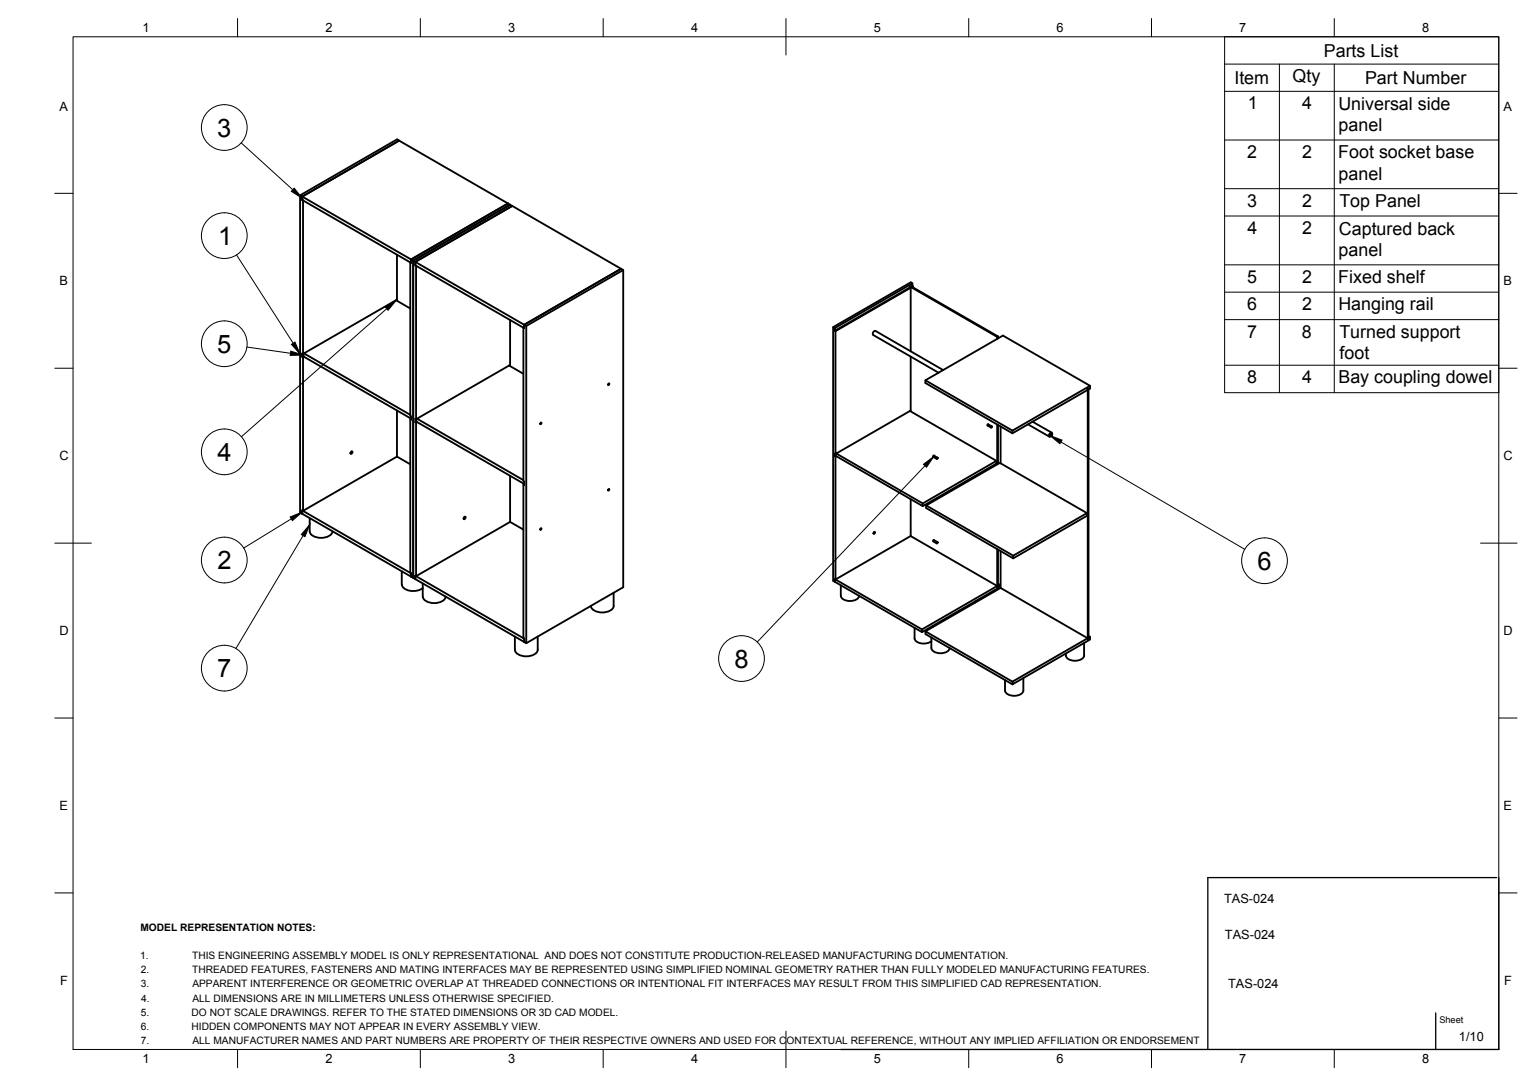
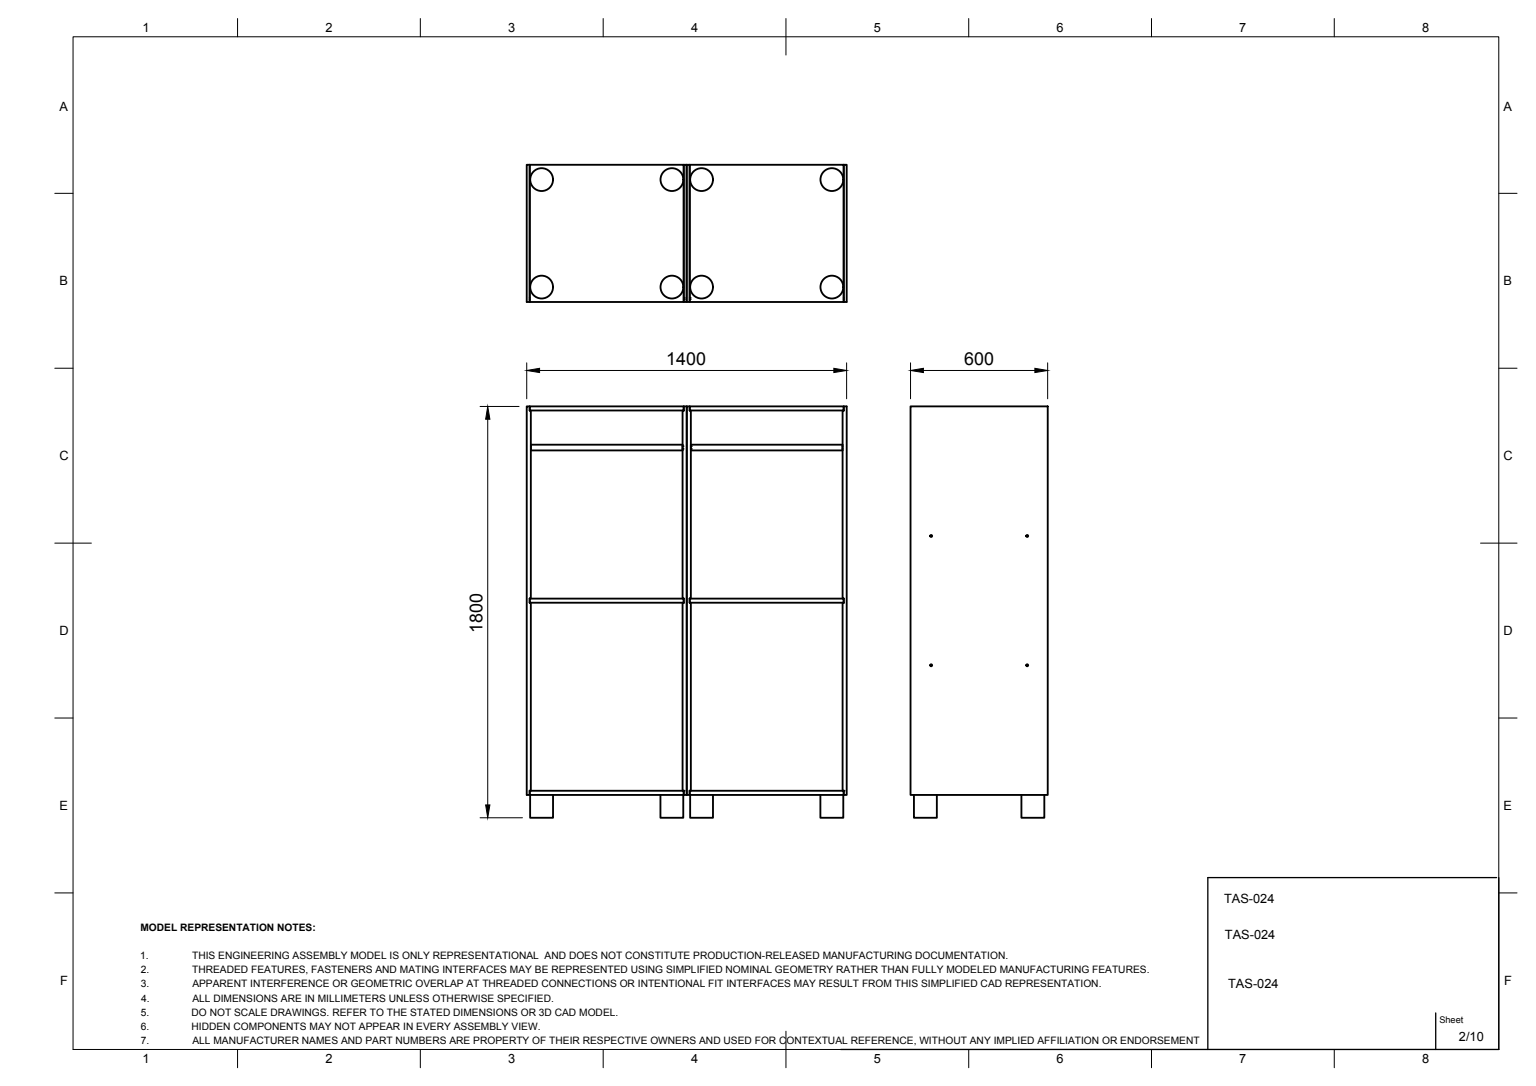
ISO-10303-21;
HEADER;
/* Generated by software containing ST-Developer
 * from STEP Tools, Inc. (www.steptools.com) 
 */

FILE_DESCRIPTION(
/* description */ (''),
/* implementation_level */ '2;1');

FILE_NAME(
/* name */ 'TAS-024.step',
/* time_stamp */ '2026-11-15T17:53:25-08:00',
/* author */ (''),
/* organization */ (''),
/* preprocessor_version */ 'ST-DEVELOPER v20.2',
/* originating_system */ 'Autodesk Translation Framework v15.17.0.0',
/* authorisation */ '');

FILE_SCHEMA (('AUTOMOTIVE_DESIGN { 1 0 10303 214 3 1 1 }'));
ENDSEC;

DATA;
#10=MECHANICAL_DESIGN_GEOMETRIC_PRESENTATION_REPRESENTATION('',(#131,#132,
#133,#134,#135,#136,#137,#138),#2673);
#11=ITEM_DEFINED_TRANSFORMATION($,$,#1615,#1744);
#12=ITEM_DEFINED_TRANSFORMATION($,$,#1662,#1745);
#13=ITEM_DEFINED_TRANSFORMATION($,$,#1689,#1746);
#14=ITEM_DEFINED_TRANSFORMATION($,$,#1700,#1747);
#15=ITEM_DEFINED_TRANSFORMATION($,$,#1707,#1748);
#16=ITEM_DEFINED_TRANSFORMATION($,$,#1714,#1749);
#17=ITEM_DEFINED_TRANSFORMATION($,$,#1728,#1750);
#18=ITEM_DEFINED_TRANSFORMATION($,$,#1738,#1751);
#19=ITEM_DEFINED_TRANSFORMATION($,$,#1615,#1752);
#20=ITEM_DEFINED_TRANSFORMATION($,$,#1728,#1753);
#21=ITEM_DEFINED_TRANSFORMATION($,$,#1728,#1754);
#22=ITEM_DEFINED_TRANSFORMATION($,$,#1728,#1755);
#23=ITEM_DEFINED_TRANSFORMATION($,$,#1615,#1756);
#24=ITEM_DEFINED_TRANSFORMATION($,$,#1615,#1757);
#25=ITEM_DEFINED_TRANSFORMATION($,$,#1662,#1758);
#26=ITEM_DEFINED_TRANSFORMATION($,$,#1689,#1759);
#27=ITEM_DEFINED_TRANSFORMATION($,$,#1700,#1760);
#28=ITEM_DEFINED_TRANSFORMATION($,$,#1707,#1761);
#29=ITEM_DEFINED_TRANSFORMATION($,$,#1714,#1762);
#30=ITEM_DEFINED_TRANSFORMATION($,$,#1728,#1763);
#31=ITEM_DEFINED_TRANSFORMATION($,$,#1728,#1764);
#32=ITEM_DEFINED_TRANSFORMATION($,$,#1728,#1765);
#33=ITEM_DEFINED_TRANSFORMATION($,$,#1728,#1766);
#34=ITEM_DEFINED_TRANSFORMATION($,$,#1738,#1767);
#35=ITEM_DEFINED_TRANSFORMATION($,$,#1738,#1768);
#36=ITEM_DEFINED_TRANSFORMATION($,$,#1738,#1769);
#37=(
REPRESENTATION_RELATIONSHIP($,$,#2723,#2722)
REPRESENTATION_RELATIONSHIP_WITH_TRANSFORMATION(#11)
SHAPE_REPRESENTATION_RELATIONSHIP()
);
#38=(
REPRESENTATION_RELATIONSHIP($,$,#2724,#2722)
REPRESENTATION_RELATIONSHIP_WITH_TRANSFORMATION(#12)
SHAPE_REPRESENTATION_RELATIONSHIP()
);
#39=(
REPRESENTATION_RELATIONSHIP($,$,#2725,#2722)
REPRESENTATION_RELATIONSHIP_WITH_TRANSFORMATION(#13)
SHAPE_REPRESENTATION_RELATIONSHIP()
);
#40=(
REPRESENTATION_RELATIONSHIP($,$,#2726,#2722)
REPRESENTATION_RELATIONSHIP_WITH_TRANSFORMATION(#14)
SHAPE_REPRESENTATION_RELATIONSHIP()
);
#41=(
REPRESENTATION_RELATIONSHIP($,$,#2727,#2722)
REPRESENTATION_RELATIONSHIP_WITH_TRANSFORMATION(#15)
SHAPE_REPRESENTATION_RELATIONSHIP()
);
#42=(
REPRESENTATION_RELATIONSHIP($,$,#2728,#2722)
REPRESENTATION_RELATIONSHIP_WITH_TRANSFORMATION(#16)
SHAPE_REPRESENTATION_RELATIONSHIP()
);
#43=(
REPRESENTATION_RELATIONSHIP($,$,#2729,#2722)
REPRESENTATION_RELATIONSHIP_WITH_TRANSFORMATION(#17)
SHAPE_REPRESENTATION_RELATIONSHIP()
);
#44=(
REPRESENTATION_RELATIONSHIP($,$,#2730,#2722)
REPRESENTATION_RELATIONSHIP_WITH_TRANSFORMATION(#18)
SHAPE_REPRESENTATION_RELATIONSHIP()
);
#45=(
REPRESENTATION_RELATIONSHIP($,$,#2723,#2722)
REPRESENTATION_RELATIONSHIP_WITH_TRANSFORMATION(#19)
SHAPE_REPRESENTATION_RELATIONSHIP()
);
#46=(
REPRESENTATION_RELATIONSHIP($,$,#2729,#2722)
REPRESENTATION_RELATIONSHIP_WITH_TRANSFORMATION(#20)
SHAPE_REPRESENTATION_RELATIONSHIP()
);
#47=(
REPRESENTATION_RELATIONSHIP($,$,#2729,#2722)
REPRESENTATION_RELATIONSHIP_WITH_TRANSFORMATION(#21)
SHAPE_REPRESENTATION_RELATIONSHIP()
);
#48=(
REPRESENTATION_RELATIONSHIP($,$,#2729,#2722)
REPRESENTATION_RELATIONSHIP_WITH_TRANSFORMATION(#22)
SHAPE_REPRESENTATION_RELATIONSHIP()
);
#49=(
REPRESENTATION_RELATIONSHIP($,$,#2723,#2722)
REPRESENTATION_RELATIONSHIP_WITH_TRANSFORMATION(#23)
SHAPE_REPRESENTATION_RELATIONSHIP()
);
#50=(
REPRESENTATION_RELATIONSHIP($,$,#2723,#2722)
REPRESENTATION_RELATIONSHIP_WITH_TRANSFORMATION(#24)
SHAPE_REPRESENTATION_RELATIONSHIP()
);
#51=(
REPRESENTATION_RELATIONSHIP($,$,#2724,#2722)
REPRESENTATION_RELATIONSHIP_WITH_TRANSFORMATION(#25)
SHAPE_REPRESENTATION_RELATIONSHIP()
);
#52=(
REPRESENTATION_RELATIONSHIP($,$,#2725,#2722)
REPRESENTATION_RELATIONSHIP_WITH_TRANSFORMATION(#26)
SHAPE_REPRESENTATION_RELATIONSHIP()
);
#53=(
REPRESENTATION_RELATIONSHIP($,$,#2726,#2722)
REPRESENTATION_RELATIONSHIP_WITH_TRANSFORMATION(#27)
SHAPE_REPRESENTATION_RELATIONSHIP()
);
#54=(
REPRESENTATION_RELATIONSHIP($,$,#2727,#2722)
REPRESENTATION_RELATIONSHIP_WITH_TRANSFORMATION(#28)
SHAPE_REPRESENTATION_RELATIONSHIP()
);
#55=(
REPRESENTATION_RELATIONSHIP($,$,#2728,#2722)
REPRESENTATION_RELATIONSHIP_WITH_TRANSFORMATION(#29)
SHAPE_REPRESENTATION_RELATIONSHIP()
);
#56=(
REPRESENTATION_RELATIONSHIP($,$,#2729,#2722)
REPRESENTATION_RELATIONSHIP_WITH_TRANSFORMATION(#30)
SHAPE_REPRESENTATION_RELATIONSHIP()
);
#57=(
REPRESENTATION_RELATIONSHIP($,$,#2729,#2722)
REPRESENTATION_RELATIONSHIP_WITH_TRANSFORMATION(#31)
SHAPE_REPRESENTATION_RELATIONSHIP()
);
#58=(
REPRESENTATION_RELATIONSHIP($,$,#2729,#2722)
REPRESENTATION_RELATIONSHIP_WITH_TRANSFORMATION(#32)
SHAPE_REPRESENTATION_RELATIONSHIP()
);
#59=(
REPRESENTATION_RELATIONSHIP($,$,#2729,#2722)
REPRESENTATION_RELATIONSHIP_WITH_TRANSFORMATION(#33)
SHAPE_REPRESENTATION_RELATIONSHIP()
);
#60=(
REPRESENTATION_RELATIONSHIP($,$,#2730,#2722)
REPRESENTATION_RELATIONSHIP_WITH_TRANSFORMATION(#34)
SHAPE_REPRESENTATION_RELATIONSHIP()
);
#61=(
REPRESENTATION_RELATIONSHIP($,$,#2730,#2722)
REPRESENTATION_RELATIONSHIP_WITH_TRANSFORMATION(#35)
SHAPE_REPRESENTATION_RELATIONSHIP()
);
#62=(
REPRESENTATION_RELATIONSHIP($,$,#2730,#2722)
REPRESENTATION_RELATIONSHIP_WITH_TRANSFORMATION(#36)
SHAPE_REPRESENTATION_RELATIONSHIP()
);
#63=CONTEXT_DEPENDENT_SHAPE_REPRESENTATION(#37,#2696);
#64=CONTEXT_DEPENDENT_SHAPE_REPRESENTATION(#38,#2697);
#65=CONTEXT_DEPENDENT_SHAPE_REPRESENTATION(#39,#2698);
#66=CONTEXT_DEPENDENT_SHAPE_REPRESENTATION(#40,#2699);
#67=CONTEXT_DEPENDENT_SHAPE_REPRESENTATION(#41,#2700);
#68=CONTEXT_DEPENDENT_SHAPE_REPRESENTATION(#42,#2701);
#69=CONTEXT_DEPENDENT_SHAPE_REPRESENTATION(#43,#2702);
#70=CONTEXT_DEPENDENT_SHAPE_REPRESENTATION(#44,#2703);
#71=CONTEXT_DEPENDENT_SHAPE_REPRESENTATION(#45,#2704);
#72=CONTEXT_DEPENDENT_SHAPE_REPRESENTATION(#46,#2705);
#73=CONTEXT_DEPENDENT_SHAPE_REPRESENTATION(#47,#2706);
#74=CONTEXT_DEPENDENT_SHAPE_REPRESENTATION(#48,#2707);
#75=CONTEXT_DEPENDENT_SHAPE_REPRESENTATION(#49,#2708);
#76=CONTEXT_DEPENDENT_SHAPE_REPRESENTATION(#50,#2709);
#77=CONTEXT_DEPENDENT_SHAPE_REPRESENTATION(#51,#2710);
#78=CONTEXT_DEPENDENT_SHAPE_REPRESENTATION(#52,#2711);
#79=CONTEXT_DEPENDENT_SHAPE_REPRESENTATION(#53,#2712);
#80=CONTEXT_DEPENDENT_SHAPE_REPRESENTATION(#54,#2713);
#81=CONTEXT_DEPENDENT_SHAPE_REPRESENTATION(#55,#2714);
#82=CONTEXT_DEPENDENT_SHAPE_REPRESENTATION(#56,#2715);
#83=CONTEXT_DEPENDENT_SHAPE_REPRESENTATION(#57,#2716);
#84=CONTEXT_DEPENDENT_SHAPE_REPRESENTATION(#58,#2717);
#85=CONTEXT_DEPENDENT_SHAPE_REPRESENTATION(#59,#2718);
#86=CONTEXT_DEPENDENT_SHAPE_REPRESENTATION(#60,#2719);
#87=CONTEXT_DEPENDENT_SHAPE_REPRESENTATION(#61,#2720);
#88=CONTEXT_DEPENDENT_SHAPE_REPRESENTATION(#62,#2721);
#89=NEXT_ASSEMBLY_USAGE_OCCURRENCE('Universal side panel:1',
'Universal side panel:1','Universal side panel:1',#2732,#2733,
'Universal side panel:1');
#90=NEXT_ASSEMBLY_USAGE_OCCURRENCE('Foot socket base panel:1',
'Foot socket base panel:1','Foot socket base panel:1',#2732,#2734,
'Foot socket base panel:1');
#91=NEXT_ASSEMBLY_USAGE_OCCURRENCE('Top panel:1','Top panel:1',
'Top panel:1',#2732,#2735,'Top panel:1');
#92=NEXT_ASSEMBLY_USAGE_OCCURRENCE('Captured back panel:1',
'Captured back panel:1','Captured back panel:1',#2732,#2736,
'Captured back panel:1');
#93=NEXT_ASSEMBLY_USAGE_OCCURRENCE('Fixed shelf:1','Fixed shelf:1',
'Fixed shelf:1',#2732,#2737,'Fixed shelf:1');
#94=NEXT_ASSEMBLY_USAGE_OCCURRENCE('Hanging rail:1','Hanging rail:1',
'Hanging rail:1',#2732,#2738,'Hanging rail:1');
#95=NEXT_ASSEMBLY_USAGE_OCCURRENCE('Turned support foot:1',
'Turned support foot:1','Turned support foot:1',#2732,#2739,
'Turned support foot:1');
#96=NEXT_ASSEMBLY_USAGE_OCCURRENCE('Bay coupling dowel:1',
'Bay coupling dowel:1','Bay coupling dowel:1',#2732,#2740,
'Bay coupling dowel:1');
#97=NEXT_ASSEMBLY_USAGE_OCCURRENCE('Universal side panel:2',
'Universal side panel:2','Universal side panel:2',#2732,#2733,
'Universal side panel:2');
#98=NEXT_ASSEMBLY_USAGE_OCCURRENCE('Turned support foot:2',
'Turned support foot:2','Turned support foot:2',#2732,#2739,
'Turned support foot:2');
#99=NEXT_ASSEMBLY_USAGE_OCCURRENCE('Turned support foot:3',
'Turned support foot:3','Turned support foot:3',#2732,#2739,
'Turned support foot:3');
#100=NEXT_ASSEMBLY_USAGE_OCCURRENCE('Turned support foot:4',
'Turned support foot:4','Turned support foot:4',#2732,#2739,
'Turned support foot:4');
#101=NEXT_ASSEMBLY_USAGE_OCCURRENCE('Universal side panel:3',
'Universal side panel:3','Universal side panel:3',#2732,#2733,
'Universal side panel:3');
#102=NEXT_ASSEMBLY_USAGE_OCCURRENCE('Universal side panel:4',
'Universal side panel:4','Universal side panel:4',#2732,#2733,
'Universal side panel:4');
#103=NEXT_ASSEMBLY_USAGE_OCCURRENCE('Foot socket base panel:2',
'Foot socket base panel:2','Foot socket base panel:2',#2732,#2734,
'Foot socket base panel:2');
#104=NEXT_ASSEMBLY_USAGE_OCCURRENCE('Top panel:2','Top panel:2',
'Top panel:2',#2732,#2735,'Top panel:2');
#105=NEXT_ASSEMBLY_USAGE_OCCURRENCE('Captured back panel:2',
'Captured back panel:2','Captured back panel:2',#2732,#2736,
'Captured back panel:2');
#106=NEXT_ASSEMBLY_USAGE_OCCURRENCE('Fixed shelf:2','Fixed shelf:2',
'Fixed shelf:2',#2732,#2737,'Fixed shelf:2');
#107=NEXT_ASSEMBLY_USAGE_OCCURRENCE('Hanging rail:2','Hanging rail:2',
'Hanging rail:2',#2732,#2738,'Hanging rail:2');
#108=NEXT_ASSEMBLY_USAGE_OCCURRENCE('Turned support foot:5',
'Turned support foot:5','Turned support foot:5',#2732,#2739,
'Turned support foot:5');
#109=NEXT_ASSEMBLY_USAGE_OCCURRENCE('Turned support foot:6',
'Turned support foot:6','Turned support foot:6',#2732,#2739,
'Turned support foot:6');
#110=NEXT_ASSEMBLY_USAGE_OCCURRENCE('Turned support foot:7',
'Turned support foot:7','Turned support foot:7',#2732,#2739,
'Turned support foot:7');
#111=NEXT_ASSEMBLY_USAGE_OCCURRENCE('Turned support foot:8',
'Turned support foot:8','Turned support foot:8',#2732,#2739,
'Turned support foot:8');
#112=NEXT_ASSEMBLY_USAGE_OCCURRENCE('Bay coupling dowel:2',
'Bay coupling dowel:2','Bay coupling dowel:2',#2732,#2740,
'Bay coupling dowel:2');
#113=NEXT_ASSEMBLY_USAGE_OCCURRENCE('Bay coupling dowel:3',
'Bay coupling dowel:3','Bay coupling dowel:3',#2732,#2740,
'Bay coupling dowel:3');
#114=NEXT_ASSEMBLY_USAGE_OCCURRENCE('Bay coupling dowel:4',
'Bay coupling dowel:4','Bay coupling dowel:4',#2732,#2740,
'Bay coupling dowel:4');
#115=SHAPE_REPRESENTATION_RELATIONSHIP('SRR','None',#2723,#123);
#116=SHAPE_REPRESENTATION_RELATIONSHIP('SRR','None',#2724,#124);
#117=SHAPE_REPRESENTATION_RELATIONSHIP('SRR','None',#2725,#125);
#118=SHAPE_REPRESENTATION_RELATIONSHIP('SRR','None',#2726,#126);
#119=SHAPE_REPRESENTATION_RELATIONSHIP('SRR','None',#2727,#127);
#120=SHAPE_REPRESENTATION_RELATIONSHIP('SRR','None',#2728,#128);
#121=SHAPE_REPRESENTATION_RELATIONSHIP('SRR','None',#2729,#129);
#122=SHAPE_REPRESENTATION_RELATIONSHIP('SRR','None',#2730,#130);
#123=ADVANCED_BREP_SHAPE_REPRESENTATION('',(#139),#2665);
#124=ADVANCED_BREP_SHAPE_REPRESENTATION('',(#140),#2666);
#125=ADVANCED_BREP_SHAPE_REPRESENTATION('',(#141),#2667);
#126=ADVANCED_BREP_SHAPE_REPRESENTATION('',(#142),#2668);
#127=ADVANCED_BREP_SHAPE_REPRESENTATION('',(#143),#2669);
#128=ADVANCED_BREP_SHAPE_REPRESENTATION('',(#144),#2670);
#129=ADVANCED_BREP_SHAPE_REPRESENTATION('',(#145),#2671);
#130=ADVANCED_BREP_SHAPE_REPRESENTATION('',(#146),#2672);
#131=STYLED_ITEM('',(#2772),#139);
#132=STYLED_ITEM('',(#2773),#140);
#133=STYLED_ITEM('',(#2774),#141);
#134=STYLED_ITEM('',(#2775),#142);
#135=STYLED_ITEM('',(#2776),#143);
#136=STYLED_ITEM('',(#2777),#144);
#137=STYLED_ITEM('',(#2778),#145);
#138=STYLED_ITEM('',(#2779),#146);
#139=MANIFOLD_SOLID_BREP('Body1',#1517);
#140=MANIFOLD_SOLID_BREP('Body1',#1518);
#141=MANIFOLD_SOLID_BREP('Body1',#1519);
#142=MANIFOLD_SOLID_BREP('Body1',#1520);
#143=MANIFOLD_SOLID_BREP('Body1',#1521);
#144=MANIFOLD_SOLID_BREP('Body1',#1522);
#145=MANIFOLD_SOLID_BREP('Body1',#1523);
#146=MANIFOLD_SOLID_BREP('Body1',#1524);
#147=FACE_BOUND('',#342,.T.);
#148=FACE_BOUND('',#349,.T.);
#149=FACE_BOUND('',#357,.T.);
#150=FACE_BOUND('',#358,.T.);
#151=FACE_BOUND('',#359,.T.);
#152=FACE_BOUND('',#360,.T.);
#153=FACE_BOUND('',#380,.T.);
#154=FACE_BOUND('',#381,.T.);
#155=FACE_BOUND('',#382,.T.);
#156=FACE_BOUND('',#383,.T.);
#157=FACE_BOUND('',#412,.T.);
#158=FACE_BOUND('',#414,.T.);
#159=FACE_BOUND('',#419,.T.);
#160=PLANE('',#1619);
#161=PLANE('',#1623);
#162=PLANE('',#1627);
#163=PLANE('',#1631);
#164=PLANE('',#1635);
#165=PLANE('',#1639);
#166=PLANE('',#1640);
#167=PLANE('',#1641);
#168=PLANE('',#1642);
#169=PLANE('',#1643);
#170=PLANE('',#1644);
#171=PLANE('',#1645);
#172=PLANE('',#1646);
#173=PLANE('',#1647);
#174=PLANE('',#1648);
#175=PLANE('',#1649);
#176=PLANE('',#1650);
#177=PLANE('',#1651);
#178=PLANE('',#1652);
#179=PLANE('',#1653);
#180=PLANE('',#1654);
#181=PLANE('',#1655);
#182=PLANE('',#1656);
#183=PLANE('',#1657);
#184=PLANE('',#1658);
#185=PLANE('',#1659);
#186=PLANE('',#1660);
#187=PLANE('',#1661);
#188=PLANE('',#1666);
#189=PLANE('',#1670);
#190=PLANE('',#1674);
#191=PLANE('',#1678);
#192=PLANE('',#1679);
#193=PLANE('',#1680);
#194=PLANE('',#1681);
#195=PLANE('',#1682);
#196=PLANE('',#1683);
#197=PLANE('',#1684);
#198=PLANE('',#1685);
#199=PLANE('',#1686);
#200=PLANE('',#1687);
#201=PLANE('',#1688);
#202=PLANE('',#1690);
#203=PLANE('',#1691);
#204=PLANE('',#1692);
#205=PLANE('',#1693);
#206=PLANE('',#1694);
#207=PLANE('',#1695);
#208=PLANE('',#1696);
#209=PLANE('',#1697);
#210=PLANE('',#1698);
#211=PLANE('',#1699);
#212=PLANE('',#1701);
#213=PLANE('',#1702);
#214=PLANE('',#1703);
#215=PLANE('',#1704);
#216=PLANE('',#1705);
#217=PLANE('',#1706);
#218=PLANE('',#1708);
#219=PLANE('',#1709);
#220=PLANE('',#1710);
#221=PLANE('',#1711);
#222=PLANE('',#1712);
#223=PLANE('',#1713);
#224=PLANE('',#1718);
#225=PLANE('',#1722);
#226=PLANE('',#1726);
#227=PLANE('',#1727);
#228=PLANE('',#1732);
#229=PLANE('',#1736);
#230=PLANE('',#1737);
#231=PLANE('',#1742);
#232=PLANE('',#1743);
#233=FACE_OUTER_BOUND('',#322,.T.);
#234=FACE_OUTER_BOUND('',#323,.T.);
#235=FACE_OUTER_BOUND('',#324,.T.);
#236=FACE_OUTER_BOUND('',#325,.T.);
#237=FACE_OUTER_BOUND('',#326,.T.);
#238=FACE_OUTER_BOUND('',#327,.T.);
#239=FACE_OUTER_BOUND('',#328,.T.);
#240=FACE_OUTER_BOUND('',#329,.T.);
#241=FACE_OUTER_BOUND('',#330,.T.);
#242=FACE_OUTER_BOUND('',#331,.T.);
#243=FACE_OUTER_BOUND('',#332,.T.);
#244=FACE_OUTER_BOUND('',#333,.T.);
#245=FACE_OUTER_BOUND('',#334,.T.);
#246=FACE_OUTER_BOUND('',#335,.T.);
#247=FACE_OUTER_BOUND('',#336,.T.);
#248=FACE_OUTER_BOUND('',#337,.T.);
#249=FACE_OUTER_BOUND('',#338,.T.);
#250=FACE_OUTER_BOUND('',#339,.T.);
#251=FACE_OUTER_BOUND('',#340,.T.);
#252=FACE_OUTER_BOUND('',#341,.T.);
#253=FACE_OUTER_BOUND('',#343,.T.);
#254=FACE_OUTER_BOUND('',#344,.T.);
#255=FACE_OUTER_BOUND('',#345,.T.);
#256=FACE_OUTER_BOUND('',#346,.T.);
#257=FACE_OUTER_BOUND('',#347,.T.);
#258=FACE_OUTER_BOUND('',#348,.T.);
#259=FACE_OUTER_BOUND('',#350,.T.);
#260=FACE_OUTER_BOUND('',#351,.T.);
#261=FACE_OUTER_BOUND('',#352,.T.);
#262=FACE_OUTER_BOUND('',#353,.T.);
#263=FACE_OUTER_BOUND('',#354,.T.);
#264=FACE_OUTER_BOUND('',#355,.T.);
#265=FACE_OUTER_BOUND('',#356,.T.);
#266=FACE_OUTER_BOUND('',#361,.T.);
#267=FACE_OUTER_BOUND('',#362,.T.);
#268=FACE_OUTER_BOUND('',#363,.T.);
#269=FACE_OUTER_BOUND('',#364,.T.);
#270=FACE_OUTER_BOUND('',#365,.T.);
#271=FACE_OUTER_BOUND('',#366,.T.);
#272=FACE_OUTER_BOUND('',#367,.T.);
#273=FACE_OUTER_BOUND('',#368,.T.);
#274=FACE_OUTER_BOUND('',#369,.T.);
#275=FACE_OUTER_BOUND('',#370,.T.);
#276=FACE_OUTER_BOUND('',#371,.T.);
#277=FACE_OUTER_BOUND('',#372,.T.);
#278=FACE_OUTER_BOUND('',#373,.T.);
#279=FACE_OUTER_BOUND('',#374,.T.);
#280=FACE_OUTER_BOUND('',#375,.T.);
#281=FACE_OUTER_BOUND('',#376,.T.);
#282=FACE_OUTER_BOUND('',#377,.T.);
#283=FACE_OUTER_BOUND('',#378,.T.);
#284=FACE_OUTER_BOUND('',#379,.T.);
#285=FACE_OUTER_BOUND('',#384,.T.);
#286=FACE_OUTER_BOUND('',#385,.T.);
#287=FACE_OUTER_BOUND('',#386,.T.);
#288=FACE_OUTER_BOUND('',#387,.T.);
#289=FACE_OUTER_BOUND('',#388,.T.);
#290=FACE_OUTER_BOUND('',#389,.T.);
#291=FACE_OUTER_BOUND('',#390,.T.);
#292=FACE_OUTER_BOUND('',#391,.T.);
#293=FACE_OUTER_BOUND('',#392,.T.);
#294=FACE_OUTER_BOUND('',#393,.T.);
#295=FACE_OUTER_BOUND('',#394,.T.);
#296=FACE_OUTER_BOUND('',#395,.T.);
#297=FACE_OUTER_BOUND('',#396,.T.);
#298=FACE_OUTER_BOUND('',#397,.T.);
#299=FACE_OUTER_BOUND('',#398,.T.);
#300=FACE_OUTER_BOUND('',#399,.T.);
#301=FACE_OUTER_BOUND('',#400,.T.);
#302=FACE_OUTER_BOUND('',#401,.T.);
#303=FACE_OUTER_BOUND('',#402,.T.);
#304=FACE_OUTER_BOUND('',#403,.T.);
#305=FACE_OUTER_BOUND('',#404,.T.);
#306=FACE_OUTER_BOUND('',#405,.T.);
#307=FACE_OUTER_BOUND('',#406,.T.);
#308=FACE_OUTER_BOUND('',#407,.T.);
#309=FACE_OUTER_BOUND('',#408,.T.);
#310=FACE_OUTER_BOUND('',#409,.T.);
#311=FACE_OUTER_BOUND('',#410,.T.);
#312=FACE_OUTER_BOUND('',#411,.T.);
#313=FACE_OUTER_BOUND('',#413,.T.);
#314=FACE_OUTER_BOUND('',#415,.T.);
#315=FACE_OUTER_BOUND('',#416,.T.);
#316=FACE_OUTER_BOUND('',#417,.T.);
#317=FACE_OUTER_BOUND('',#418,.T.);
#318=FACE_OUTER_BOUND('',#420,.T.);
#319=FACE_OUTER_BOUND('',#421,.T.);
#320=FACE_OUTER_BOUND('',#422,.T.);
#321=FACE_OUTER_BOUND('',#423,.T.);
#322=EDGE_LOOP('',(#1052,#1053,#1054,#1055));
#323=EDGE_LOOP('',(#1056));
#324=EDGE_LOOP('',(#1057,#1058,#1059,#1060));
#325=EDGE_LOOP('',(#1061));
#326=EDGE_LOOP('',(#1062,#1063,#1064,#1065));
#327=EDGE_LOOP('',(#1066));
#328=EDGE_LOOP('',(#1067,#1068,#1069,#1070));
#329=EDGE_LOOP('',(#1071));
#330=EDGE_LOOP('',(#1072,#1073,#1074,#1075));
#331=EDGE_LOOP('',(#1076));
#332=EDGE_LOOP('',(#1077,#1078,#1079,#1080));
#333=EDGE_LOOP('',(#1081));
#334=EDGE_LOOP('',(#1082,#1083,#1084,#1085));
#335=EDGE_LOOP('',(#1086,#1087,#1088,#1089));
#336=EDGE_LOOP('',(#1090,#1091,#1092,#1093));
#337=EDGE_LOOP('',(#1094,#1095,#1096,#1097));
#338=EDGE_LOOP('',(#1098,#1099,#1100,#1101,#1102,#1103,#1104,#1105,#1106,
#1107,#1108,#1109,#1110,#1111,#1112,#1113,#1114,#1115,#1116,#1117));
#339=EDGE_LOOP('',(#1118,#1119,#1120,#1121));
#340=EDGE_LOOP('',(#1122,#1123,#1124,#1125));
#341=EDGE_LOOP('',(#1126,#1127,#1128,#1129));
#342=EDGE_LOOP('',(#1130));
#343=EDGE_LOOP('',(#1131,#1132,#1133,#1134));
#344=EDGE_LOOP('',(#1135,#1136,#1137,#1138));
#345=EDGE_LOOP('',(#1139,#1140,#1141,#1142));
#346=EDGE_LOOP('',(#1143,#1144,#1145,#1146));
#347=EDGE_LOOP('',(#1147,#1148,#1149,#1150));
#348=EDGE_LOOP('',(#1151,#1152,#1153,#1154));
#349=EDGE_LOOP('',(#1155));
#350=EDGE_LOOP('',(#1156,#1157,#1158,#1159));
#351=EDGE_LOOP('',(#1160,#1161,#1162,#1163));
#352=EDGE_LOOP('',(#1164,#1165,#1166,#1167));
#353=EDGE_LOOP('',(#1168,#1169,#1170,#1171,#1172,#1173,#1174,#1175,#1176,
#1177,#1178,#1179));
#354=EDGE_LOOP('',(#1180,#1181,#1182,#1183));
#355=EDGE_LOOP('',(#1184,#1185,#1186,#1187,#1188,#1189,#1190,#1191,#1192,
#1193,#1194,#1195));
#356=EDGE_LOOP('',(#1196,#1197,#1198,#1199));
#357=EDGE_LOOP('',(#1200));
#358=EDGE_LOOP('',(#1201));
#359=EDGE_LOOP('',(#1202));
#360=EDGE_LOOP('',(#1203));
#361=EDGE_LOOP('',(#1204,#1205,#1206,#1207));
#362=EDGE_LOOP('',(#1208,#1209,#1210,#1211));
#363=EDGE_LOOP('',(#1212));
#364=EDGE_LOOP('',(#1213,#1214,#1215,#1216));
#365=EDGE_LOOP('',(#1217));
#366=EDGE_LOOP('',(#1218,#1219,#1220,#1221));
#367=EDGE_LOOP('',(#1222));
#368=EDGE_LOOP('',(#1223,#1224,#1225,#1226));
#369=EDGE_LOOP('',(#1227));
#370=EDGE_LOOP('',(#1228,#1229,#1230,#1231));
#371=EDGE_LOOP('',(#1232,#1233,#1234,#1235));
#372=EDGE_LOOP('',(#1236,#1237,#1238,#1239));
#373=EDGE_LOOP('',(#1240,#1241,#1242,#1243,#1244,#1245,#1246,#1247));
#374=EDGE_LOOP('',(#1248,#1249,#1250,#1251));
#375=EDGE_LOOP('',(#1252,#1253,#1254,#1255));
#376=EDGE_LOOP('',(#1256,#1257,#1258,#1259));
#377=EDGE_LOOP('',(#1260,#1261,#1262,#1263,#1264,#1265,#1266,#1267));
#378=EDGE_LOOP('',(#1268,#1269,#1270,#1271));
#379=EDGE_LOOP('',(#1272,#1273,#1274,#1275));
#380=EDGE_LOOP('',(#1276));
#381=EDGE_LOOP('',(#1277));
#382=EDGE_LOOP('',(#1278));
#383=EDGE_LOOP('',(#1279));
#384=EDGE_LOOP('',(#1280,#1281,#1282,#1283));
#385=EDGE_LOOP('',(#1284,#1285,#1286,#1287));
#386=EDGE_LOOP('',(#1288,#1289,#1290,#1291));
#387=EDGE_LOOP('',(#1292,#1293,#1294,#1295,#1296,#1297,#1298,#1299));
#388=EDGE_LOOP('',(#1300,#1301,#1302,#1303));
#389=EDGE_LOOP('',(#1304,#1305,#1306,#1307));
#390=EDGE_LOOP('',(#1308,#1309,#1310,#1311));
#391=EDGE_LOOP('',(#1312,#1313,#1314,#1315,#1316,#1317,#1318,#1319));
#392=EDGE_LOOP('',(#1320,#1321,#1322,#1323));
#393=EDGE_LOOP('',(#1324,#1325,#1326,#1327));
#394=EDGE_LOOP('',(#1328,#1329,#1330,#1331));
#395=EDGE_LOOP('',(#1332,#1333,#1334,#1335));
#396=EDGE_LOOP('',(#1336,#1337,#1338,#1339));
#397=EDGE_LOOP('',(#1340,#1341,#1342,#1343));
#398=EDGE_LOOP('',(#1344,#1345,#1346,#1347));
#399=EDGE_LOOP('',(#1348,#1349,#1350,#1351));
#400=EDGE_LOOP('',(#1352,#1353,#1354,#1355));
#401=EDGE_LOOP('',(#1356,#1357,#1358,#1359));
#402=EDGE_LOOP('',(#1360,#1361,#1362,#1363));
#403=EDGE_LOOP('',(#1364,#1365,#1366,#1367));
#404=EDGE_LOOP('',(#1368,#1369,#1370,#1371));
#405=EDGE_LOOP('',(#1372,#1373,#1374,#1375));
#406=EDGE_LOOP('',(#1376,#1377,#1378,#1379));
#407=EDGE_LOOP('',(#1380));
#408=EDGE_LOOP('',(#1381,#1382,#1383,#1384));
#409=EDGE_LOOP('',(#1385));
#410=EDGE_LOOP('',(#1386,#1387,#1388,#1389));
#411=EDGE_LOOP('',(#1390));
#412=EDGE_LOOP('',(#1391));
#413=EDGE_LOOP('',(#1392));
#414=EDGE_LOOP('',(#1393));
#415=EDGE_LOOP('',(#1394,#1395,#1396,#1397));
#416=EDGE_LOOP('',(#1398));
#417=EDGE_LOOP('',(#1399,#1400,#1401,#1402));
#418=EDGE_LOOP('',(#1403));
#419=EDGE_LOOP('',(#1404));
#420=EDGE_LOOP('',(#1405));
#421=EDGE_LOOP('',(#1406,#1407,#1408,#1409));
#422=EDGE_LOOP('',(#1410));
#423=EDGE_LOOP('',(#1411));
#424=LINE('',#2236,#572);
#425=LINE('',#2243,#573);
#426=LINE('',#2250,#574);
#427=LINE('',#2257,#575);
#428=LINE('',#2264,#576);
#429=LINE('',#2271,#577);
#430=LINE('',#2277,#578);
#431=LINE('',#2279,#579);
#432=LINE('',#2281,#580);
#433=LINE('',#2282,#581);
#434=LINE('',#2286,#582);
#435=LINE('',#2288,#583);
#436=LINE('',#2290,#584);
#437=LINE('',#2291,#585);
#438=LINE('',#2295,#586);
#439=LINE('',#2297,#587);
#440=LINE('',#2299,#588);
#441=LINE('',#2300,#589);
#442=LINE('',#2304,#590);
#443=LINE('',#2306,#591);
#444=LINE('',#2308,#592);
#445=LINE('',#2309,#593);
#446=LINE('',#2312,#594);
#447=LINE('',#2314,#595);
#448=LINE('',#2316,#596);
#449=LINE('',#2318,#597);
#450=LINE('',#2319,#598);
#451=LINE('',#2321,#599);
#452=LINE('',#2323,#600);
#453=LINE('',#2324,#601);
#454=LINE('',#2326,#602);
#455=LINE('',#2328,#603);
#456=LINE('',#2330,#604);
#457=LINE('',#2332,#605);
#458=LINE('',#2333,#606);
#459=LINE('',#2335,#607);
#460=LINE('',#2337,#608);
#461=LINE('',#2338,#609);
#462=LINE('',#2341,#610);
#463=LINE('',#2342,#611);
#464=LINE('',#2345,#612);
#465=LINE('',#2346,#613);
#466=LINE('',#2349,#614);
#467=LINE('',#2350,#615);
#468=LINE('',#2353,#616);
#469=LINE('',#2354,#617);
#470=LINE('',#2356,#618);
#471=LINE('',#2358,#619);
#472=LINE('',#2361,#620);
#473=LINE('',#2362,#621);
#474=LINE('',#2365,#622);
#475=LINE('',#2366,#623);
#476=LINE('',#2369,#624);
#477=LINE('',#2370,#625);
#478=LINE('',#2373,#626);
#479=LINE('',#2374,#627);
#480=LINE('',#2376,#628);
#481=LINE('',#2378,#629);
#482=LINE('',#2381,#630);
#483=LINE('',#2383,#631);
#484=LINE('',#2384,#632);
#485=LINE('',#2387,#633);
#486=LINE('',#2388,#634);
#487=LINE('',#2391,#635);
#488=LINE('',#2392,#636);
#489=LINE('',#2394,#637);
#490=LINE('',#2401,#638);
#491=LINE('',#2408,#639);
#492=LINE('',#2415,#640);
#493=LINE('',#2422,#641);
#494=LINE('',#2428,#642);
#495=LINE('',#2430,#643);
#496=LINE('',#2432,#644);
#497=LINE('',#2433,#645);
#498=LINE('',#2437,#646);
#499=LINE('',#2439,#647);
#500=LINE('',#2441,#648);
#501=LINE('',#2442,#649);
#502=LINE('',#2444,#650);
#503=LINE('',#2445,#651);
#504=LINE('',#2448,#652);
#505=LINE('',#2450,#653);
#506=LINE('',#2452,#654);
#507=LINE('',#2454,#655);
#508=LINE('',#2455,#656);
#509=LINE('',#2458,#657);
#510=LINE('',#2459,#658);
#511=LINE('',#2462,#659);
#512=LINE('',#2464,#660);
#513=LINE('',#2465,#661);
#514=LINE('',#2468,#662);
#515=LINE('',#2469,#663);
#516=LINE('',#2471,#664);
#517=LINE('',#2472,#665);
#518=LINE('',#2479,#666);
#519=LINE('',#2481,#667);
#520=LINE('',#2483,#668);
#521=LINE('',#2484,#669);
#522=LINE('',#2488,#670);
#523=LINE('',#2490,#671);
#524=LINE('',#2492,#672);
#525=LINE('',#2493,#673);
#526=LINE('',#2495,#674);
#527=LINE('',#2496,#675);
#528=LINE('',#2499,#676);
#529=LINE('',#2501,#677);
#530=LINE('',#2503,#678);
#531=LINE('',#2505,#679);
#532=LINE('',#2506,#680);
#533=LINE('',#2509,#681);
#534=LINE('',#2510,#682);
#535=LINE('',#2513,#683);
#536=LINE('',#2515,#684);
#537=LINE('',#2516,#685);
#538=LINE('',#2519,#686);
#539=LINE('',#2520,#687);
#540=LINE('',#2522,#688);
#541=LINE('',#2523,#689);
#542=LINE('',#2530,#690);
#543=LINE('',#2532,#691);
#544=LINE('',#2534,#692);
#545=LINE('',#2535,#693);
#546=LINE('',#2538,#694);
#547=LINE('',#2540,#695);
#548=LINE('',#2541,#696);
#549=LINE('',#2544,#697);
#550=LINE('',#2546,#698);
#551=LINE('',#2547,#699);
#552=LINE('',#2549,#700);
#553=LINE('',#2550,#701);
#554=LINE('',#2557,#702);
#555=LINE('',#2559,#703);
#556=LINE('',#2561,#704);
#557=LINE('',#2562,#705);
#558=LINE('',#2565,#706);
#559=LINE('',#2567,#707);
#560=LINE('',#2568,#708);
#561=LINE('',#2571,#709);
#562=LINE('',#2573,#710);
#563=LINE('',#2574,#711);
#564=LINE('',#2576,#712);
#565=LINE('',#2577,#713);
#566=LINE('',#2585,#714);
#567=LINE('',#2592,#715);
#568=LINE('',#2599,#716);
#569=LINE('',#2608,#717);
#570=LINE('',#2615,#718);
#571=LINE('',#2624,#719);
#572=VECTOR('',#1778,0.409999999999997);
#573=VECTOR('',#1787,0.409999999999997);
#574=VECTOR('',#1796,0.409999999999997);
#575=VECTOR('',#1805,0.409999999999997);
#576=VECTOR('',#1814,0.620000000000001);
#577=VECTOR('',#1823,0.620000000000005);
#578=VECTOR('',#1830,1.);
#579=VECTOR('',#1831,1.);
#580=VECTOR('',#1832,1.);
#581=VECTOR('',#1833,1.);
#582=VECTOR('',#1836,1.);
#583=VECTOR('',#1837,1.);
#584=VECTOR('',#1838,1.);
#585=VECTOR('',#1839,1.);
#586=VECTOR('',#1842,1.);
#587=VECTOR('',#1843,1.);
#588=VECTOR('',#1844,1.);
#589=VECTOR('',#1845,1.);
#590=VECTOR('',#1848,1.);
#591=VECTOR('',#1849,1.);
#592=VECTOR('',#1850,1.);
#593=VECTOR('',#1851,1.);
#594=VECTOR('',#1854,1.);
#595=VECTOR('',#1855,1.);
#596=VECTOR('',#1856,1.);
#597=VECTOR('',#1857,1.);
#598=VECTOR('',#1858,1.);
#599=VECTOR('',#1859,1.);
#600=VECTOR('',#1860,1.);
#601=VECTOR('',#1861,1.);
#602=VECTOR('',#1862,1.);
#603=VECTOR('',#1863,1.);
#604=VECTOR('',#1864,1.);
#605=VECTOR('',#1865,1.);
#606=VECTOR('',#1866,1.);
#607=VECTOR('',#1867,1.);
#608=VECTOR('',#1868,1.);
#609=VECTOR('',#1869,1.);
#610=VECTOR('',#1872,1.);
#611=VECTOR('',#1873,1.);
#612=VECTOR('',#1876,1.);
#613=VECTOR('',#1877,1.);
#614=VECTOR('',#1880,1.);
#615=VECTOR('',#1881,1.);
#616=VECTOR('',#1884,1.);
#617=VECTOR('',#1885,1.);
#618=VECTOR('',#1888,1.);
#619=VECTOR('',#1891,1.);
#620=VECTOR('',#1894,1.);
#621=VECTOR('',#1895,1.);
#622=VECTOR('',#1898,1.);
#623=VECTOR('',#1899,1.);
#624=VECTOR('',#1902,1.);
#625=VECTOR('',#1903,1.);
#626=VECTOR('',#1906,1.);
#627=VECTOR('',#1907,1.);
#628=VECTOR('',#1910,1.);
#629=VECTOR('',#1913,1.);
#630=VECTOR('',#1916,1.);
#631=VECTOR('',#1917,1.);
#632=VECTOR('',#1918,1.);
#633=VECTOR('',#1921,1.);
#634=VECTOR('',#1922,1.);
#635=VECTOR('',#1925,1.);
#636=VECTOR('',#1926,1.);
#637=VECTOR('',#1929,1.);
#638=VECTOR('',#1938,0.619999999999997);
#639=VECTOR('',#1947,0.62);
#640=VECTOR('',#1956,0.62);
#641=VECTOR('',#1965,0.619999999999997);
#642=VECTOR('',#1972,1.);
#643=VECTOR('',#1973,1.);
#644=VECTOR('',#1974,1.);
#645=VECTOR('',#1975,1.);
#646=VECTOR('',#1978,1.);
#647=VECTOR('',#1979,1.);
#648=VECTOR('',#1980,1.);
#649=VECTOR('',#1981,1.);
#650=VECTOR('',#1984,1.);
#651=VECTOR('',#1985,1.);
#652=VECTOR('',#1988,1.);
#653=VECTOR('',#1989,1.);
#654=VECTOR('',#1990,1.);
#655=VECTOR('',#1991,1.);
#656=VECTOR('',#1992,1.);
#657=VECTOR('',#1995,1.);
#658=VECTOR('',#1996,1.);
#659=VECTOR('',#1999,1.);
#660=VECTOR('',#2000,1.);
#661=VECTOR('',#2001,1.);
#662=VECTOR('',#2004,1.);
#663=VECTOR('',#2005,1.);
#664=VECTOR('',#2008,1.);
#665=VECTOR('',#2009,1.);
#666=VECTOR('',#2018,1.);
#667=VECTOR('',#2019,1.);
#668=VECTOR('',#2020,1.);
#669=VECTOR('',#2021,1.);
#670=VECTOR('',#2024,1.);
#671=VECTOR('',#2025,1.);
#672=VECTOR('',#2026,1.);
#673=VECTOR('',#2027,1.);
#674=VECTOR('',#2030,1.);
#675=VECTOR('',#2031,1.);
#676=VECTOR('',#2034,1.);
#677=VECTOR('',#2035,1.);
#678=VECTOR('',#2036,1.);
#679=VECTOR('',#2037,1.);
#680=VECTOR('',#2038,1.);
#681=VECTOR('',#2041,1.);
#682=VECTOR('',#2042,1.);
#683=VECTOR('',#2045,1.);
#684=VECTOR('',#2046,1.);
#685=VECTOR('',#2047,1.);
#686=VECTOR('',#2050,1.);
#687=VECTOR('',#2051,1.);
#688=VECTOR('',#2054,1.);
#689=VECTOR('',#2055,1.);
#690=VECTOR('',#2064,1.);
#691=VECTOR('',#2065,1.);
#692=VECTOR('',#2066,1.);
#693=VECTOR('',#2067,1.);
#694=VECTOR('',#2070,1.);
#695=VECTOR('',#2071,1.);
#696=VECTOR('',#2072,1.);
#697=VECTOR('',#2075,1.);
#698=VECTOR('',#2076,1.);
#699=VECTOR('',#2077,1.);
#700=VECTOR('',#2080,1.);
#701=VECTOR('',#2081,1.);
#702=VECTOR('',#2090,1.);
#703=VECTOR('',#2091,1.);
#704=VECTOR('',#2092,1.);
#705=VECTOR('',#2093,1.);
#706=VECTOR('',#2096,1.);
#707=VECTOR('',#2097,1.);
#708=VECTOR('',#2098,1.);
#709=VECTOR('',#2101,1.);
#710=VECTOR('',#2102,1.);
#711=VECTOR('',#2103,1.);
#712=VECTOR('',#2106,1.);
#713=VECTOR('',#2107,1.);
#714=VECTOR('',#2118,0.6);
#715=VECTOR('',#2127,0.6);
#716=VECTOR('',#2136,1.25);
#717=VECTOR('',#2149,0.6);
#718=VECTOR('',#2158,5.);
#719=VECTOR('',#2171,0.4);
#720=CIRCLE('',#1617,0.409999999999997);
#721=CIRCLE('',#1618,0.409999999999997);
#722=CIRCLE('',#1621,0.409999999999997);
#723=CIRCLE('',#1622,0.409999999999997);
#724=CIRCLE('',#1625,0.409999999999997);
#725=CIRCLE('',#1626,0.409999999999997);
#726=CIRCLE('',#1629,0.409999999999997);
#727=CIRCLE('',#1630,0.409999999999997);
#728=CIRCLE('',#1633,0.620000000000001);
#729=CIRCLE('',#1634,0.620000000000001);
#730=CIRCLE('',#1637,0.620000000000005);
#731=CIRCLE('',#1638,0.620000000000005);
#732=CIRCLE('',#1664,0.619999999999997);
#733=CIRCLE('',#1665,0.619999999999997);
#734=CIRCLE('',#1668,0.62);
#735=CIRCLE('',#1669,0.62);
#736=CIRCLE('',#1672,0.62);
#737=CIRCLE('',#1673,0.62);
#738=CIRCLE('',#1676,0.619999999999997);
#739=CIRCLE('',#1677,0.619999999999997);
#740=CIRCLE('',#1716,0.6);
#741=CIRCLE('',#1717,0.6);
#742=CIRCLE('',#1720,0.6);
#743=CIRCLE('',#1721,0.6);
#744=CIRCLE('',#1724,1.25);
#745=CIRCLE('',#1725,1.25);
#746=CIRCLE('',#1730,0.6);
#747=CIRCLE('',#1731,0.6);
#748=CIRCLE('',#1734,5.);
#749=CIRCLE('',#1735,5.);
#750=CIRCLE('',#1740,0.4);
#751=CIRCLE('',#1741,0.4);
#752=VERTEX_POINT('',#2233);
#753=VERTEX_POINT('',#2235);
#754=VERTEX_POINT('',#2240);
#755=VERTEX_POINT('',#2242);
#756=VERTEX_POINT('',#2247);
#757=VERTEX_POINT('',#2249);
#758=VERTEX_POINT('',#2254);
#759=VERTEX_POINT('',#2256);
#760=VERTEX_POINT('',#2261);
#761=VERTEX_POINT('',#2263);
#762=VERTEX_POINT('',#2268);
#763=VERTEX_POINT('',#2270);
#764=VERTEX_POINT('',#2275);
#765=VERTEX_POINT('',#2276);
#766=VERTEX_POINT('',#2278);
#767=VERTEX_POINT('',#2280);
#768=VERTEX_POINT('',#2284);
#769=VERTEX_POINT('',#2285);
#770=VERTEX_POINT('',#2287);
#771=VERTEX_POINT('',#2289);
#772=VERTEX_POINT('',#2293);
#773=VERTEX_POINT('',#2294);
#774=VERTEX_POINT('',#2296);
#775=VERTEX_POINT('',#2298);
#776=VERTEX_POINT('',#2302);
#777=VERTEX_POINT('',#2303);
#778=VERTEX_POINT('',#2305);
#779=VERTEX_POINT('',#2307);
#780=VERTEX_POINT('',#2311);
#781=VERTEX_POINT('',#2313);
#782=VERTEX_POINT('',#2315);
#783=VERTEX_POINT('',#2317);
#784=VERTEX_POINT('',#2320);
#785=VERTEX_POINT('',#2322);
#786=VERTEX_POINT('',#2325);
#787=VERTEX_POINT('',#2327);
#788=VERTEX_POINT('',#2329);
#789=VERTEX_POINT('',#2331);
#790=VERTEX_POINT('',#2334);
#791=VERTEX_POINT('',#2336);
#792=VERTEX_POINT('',#2340);
#793=VERTEX_POINT('',#2344);
#794=VERTEX_POINT('',#2348);
#795=VERTEX_POINT('',#2352);
#796=VERTEX_POINT('',#2360);
#797=VERTEX_POINT('',#2364);
#798=VERTEX_POINT('',#2368);
#799=VERTEX_POINT('',#2372);
#800=VERTEX_POINT('',#2380);
#801=VERTEX_POINT('',#2382);
#802=VERTEX_POINT('',#2386);
#803=VERTEX_POINT('',#2390);
#804=VERTEX_POINT('',#2398);
#805=VERTEX_POINT('',#2400);
#806=VERTEX_POINT('',#2405);
#807=VERTEX_POINT('',#2407);
#808=VERTEX_POINT('',#2412);
#809=VERTEX_POINT('',#2414);
#810=VERTEX_POINT('',#2419);
#811=VERTEX_POINT('',#2421);
#812=VERTEX_POINT('',#2426);
#813=VERTEX_POINT('',#2427);
#814=VERTEX_POINT('',#2429);
#815=VERTEX_POINT('',#2431);
#816=VERTEX_POINT('',#2435);
#817=VERTEX_POINT('',#2436);
#818=VERTEX_POINT('',#2438);
#819=VERTEX_POINT('',#2440);
#820=VERTEX_POINT('',#2447);
#821=VERTEX_POINT('',#2449);
#822=VERTEX_POINT('',#2451);
#823=VERTEX_POINT('',#2453);
#824=VERTEX_POINT('',#2457);
#825=VERTEX_POINT('',#2461);
#826=VERTEX_POINT('',#2463);
#827=VERTEX_POINT('',#2467);
#828=VERTEX_POINT('',#2477);
#829=VERTEX_POINT('',#2478);
#830=VERTEX_POINT('',#2480);
#831=VERTEX_POINT('',#2482);
#832=VERTEX_POINT('',#2486);
#833=VERTEX_POINT('',#2487);
#834=VERTEX_POINT('',#2489);
#835=VERTEX_POINT('',#2491);
#836=VERTEX_POINT('',#2498);
#837=VERTEX_POINT('',#2500);
#838=VERTEX_POINT('',#2502);
#839=VERTEX_POINT('',#2504);
#840=VERTEX_POINT('',#2508);
#841=VERTEX_POINT('',#2512);
#842=VERTEX_POINT('',#2514);
#843=VERTEX_POINT('',#2518);
#844=VERTEX_POINT('',#2528);
#845=VERTEX_POINT('',#2529);
#846=VERTEX_POINT('',#2531);
#847=VERTEX_POINT('',#2533);
#848=VERTEX_POINT('',#2537);
#849=VERTEX_POINT('',#2539);
#850=VERTEX_POINT('',#2543);
#851=VERTEX_POINT('',#2545);
#852=VERTEX_POINT('',#2555);
#853=VERTEX_POINT('',#2556);
#854=VERTEX_POINT('',#2558);
#855=VERTEX_POINT('',#2560);
#856=VERTEX_POINT('',#2564);
#857=VERTEX_POINT('',#2566);
#858=VERTEX_POINT('',#2570);
#859=VERTEX_POINT('',#2572);
#860=VERTEX_POINT('',#2582);
#861=VERTEX_POINT('',#2584);
#862=VERTEX_POINT('',#2589);
#863=VERTEX_POINT('',#2591);
#864=VERTEX_POINT('',#2596);
#865=VERTEX_POINT('',#2598);
#866=VERTEX_POINT('',#2605);
#867=VERTEX_POINT('',#2607);
#868=VERTEX_POINT('',#2612);
#869=VERTEX_POINT('',#2614);
#870=VERTEX_POINT('',#2621);
#871=VERTEX_POINT('',#2623);
#872=EDGE_CURVE('',#752,#752,#720,.T.);
#873=EDGE_CURVE('',#752,#753,#424,.T.);
#874=EDGE_CURVE('',#753,#753,#721,.T.);
#875=EDGE_CURVE('',#754,#754,#722,.T.);
#876=EDGE_CURVE('',#754,#755,#425,.T.);
#877=EDGE_CURVE('',#755,#755,#723,.T.);
#878=EDGE_CURVE('',#756,#756,#724,.T.);
#879=EDGE_CURVE('',#756,#757,#426,.T.);
#880=EDGE_CURVE('',#757,#757,#725,.T.);
#881=EDGE_CURVE('',#758,#758,#726,.T.);
#882=EDGE_CURVE('',#758,#759,#427,.T.);
#883=EDGE_CURVE('',#759,#759,#727,.T.);
#884=EDGE_CURVE('',#760,#760,#728,.T.);
#885=EDGE_CURVE('',#760,#761,#428,.T.);
#886=EDGE_CURVE('',#761,#761,#729,.T.);
#887=EDGE_CURVE('',#762,#762,#730,.T.);
#888=EDGE_CURVE('',#762,#763,#429,.T.);
#889=EDGE_CURVE('',#763,#763,#731,.T.);
#890=EDGE_CURVE('',#764,#765,#430,.T.);
#891=EDGE_CURVE('',#766,#764,#431,.T.);
#892=EDGE_CURVE('',#767,#766,#432,.T.);
#893=EDGE_CURVE('',#765,#767,#433,.T.);
#894=EDGE_CURVE('',#768,#769,#434,.T.);
#895=EDGE_CURVE('',#770,#768,#435,.T.);
#896=EDGE_CURVE('',#771,#770,#436,.T.);
#897=EDGE_CURVE('',#769,#771,#437,.T.);
#898=EDGE_CURVE('',#772,#773,#438,.T.);
#899=EDGE_CURVE('',#774,#772,#439,.T.);
#900=EDGE_CURVE('',#775,#774,#440,.T.);
#901=EDGE_CURVE('',#775,#773,#441,.T.);
#902=EDGE_CURVE('',#776,#777,#442,.T.);
#903=EDGE_CURVE('',#778,#776,#443,.T.);
#904=EDGE_CURVE('',#779,#778,#444,.T.);
#905=EDGE_CURVE('',#779,#777,#445,.T.);
#906=EDGE_CURVE('',#780,#768,#446,.T.);
#907=EDGE_CURVE('',#781,#780,#447,.T.);
#908=EDGE_CURVE('',#782,#781,#448,.T.);
#909=EDGE_CURVE('',#783,#782,#449,.T.);
#910=EDGE_CURVE('',#777,#783,#450,.T.);
#911=EDGE_CURVE('',#779,#784,#451,.T.);
#912=EDGE_CURVE('',#785,#784,#452,.T.);
#913=EDGE_CURVE('',#773,#785,#453,.T.);
#914=EDGE_CURVE('',#775,#786,#454,.T.);
#915=EDGE_CURVE('',#787,#786,#455,.T.);
#916=EDGE_CURVE('',#788,#787,#456,.T.);
#917=EDGE_CURVE('',#789,#788,#457,.T.);
#918=EDGE_CURVE('',#789,#766,#458,.T.);
#919=EDGE_CURVE('',#790,#764,#459,.T.);
#920=EDGE_CURVE('',#791,#790,#460,.T.);
#921=EDGE_CURVE('',#791,#770,#461,.T.);
#922=EDGE_CURVE('',#792,#783,#462,.T.);
#923=EDGE_CURVE('',#776,#792,#463,.T.);
#924=EDGE_CURVE('',#793,#769,#464,.T.);
#925=EDGE_CURVE('',#780,#793,#465,.T.);
#926=EDGE_CURVE('',#794,#792,#466,.T.);
#927=EDGE_CURVE('',#794,#778,#467,.T.);
#928=EDGE_CURVE('',#771,#795,#468,.T.);
#929=EDGE_CURVE('',#795,#793,#469,.T.);
#930=EDGE_CURVE('',#784,#794,#470,.T.);
#931=EDGE_CURVE('',#795,#791,#471,.T.);
#932=EDGE_CURVE('',#796,#785,#472,.T.);
#933=EDGE_CURVE('',#772,#796,#473,.T.);
#934=EDGE_CURVE('',#797,#765,#474,.T.);
#935=EDGE_CURVE('',#790,#797,#475,.T.);
#936=EDGE_CURVE('',#798,#796,#476,.T.);
#937=EDGE_CURVE('',#798,#774,#477,.T.);
#938=EDGE_CURVE('',#767,#799,#478,.T.);
#939=EDGE_CURVE('',#799,#797,#479,.T.);
#940=EDGE_CURVE('',#786,#798,#480,.T.);
#941=EDGE_CURVE('',#799,#789,#481,.T.);
#942=EDGE_CURVE('',#788,#800,#482,.T.);
#943=EDGE_CURVE('',#800,#801,#483,.T.);
#944=EDGE_CURVE('',#781,#801,#484,.T.);
#945=EDGE_CURVE('',#802,#787,#485,.T.);
#946=EDGE_CURVE('',#800,#802,#486,.T.);
#947=EDGE_CURVE('',#803,#782,#487,.T.);
#948=EDGE_CURVE('',#802,#803,#488,.T.);
#949=EDGE_CURVE('',#801,#803,#489,.T.);
#950=EDGE_CURVE('',#804,#804,#732,.T.);
#951=EDGE_CURVE('',#804,#805,#490,.T.);
#952=EDGE_CURVE('',#805,#805,#733,.T.);
#953=EDGE_CURVE('',#806,#806,#734,.T.);
#954=EDGE_CURVE('',#806,#807,#491,.T.);
#955=EDGE_CURVE('',#807,#807,#735,.T.);
#956=EDGE_CURVE('',#808,#808,#736,.T.);
#957=EDGE_CURVE('',#808,#809,#492,.T.);
#958=EDGE_CURVE('',#809,#809,#737,.T.);
#959=EDGE_CURVE('',#810,#810,#738,.T.);
#960=EDGE_CURVE('',#810,#811,#493,.T.);
#961=EDGE_CURVE('',#811,#811,#739,.T.);
#962=EDGE_CURVE('',#812,#813,#494,.T.);
#963=EDGE_CURVE('',#814,#812,#495,.T.);
#964=EDGE_CURVE('',#815,#814,#496,.T.);
#965=EDGE_CURVE('',#813,#815,#497,.T.);
#966=EDGE_CURVE('',#816,#817,#498,.T.);
#967=EDGE_CURVE('',#818,#816,#499,.T.);
#968=EDGE_CURVE('',#819,#818,#500,.T.);
#969=EDGE_CURVE('',#817,#819,#501,.T.);
#970=EDGE_CURVE('',#815,#818,#502,.T.);
#971=EDGE_CURVE('',#819,#814,#503,.T.);
#972=EDGE_CURVE('',#820,#812,#504,.T.);
#973=EDGE_CURVE('',#821,#820,#505,.T.);
#974=EDGE_CURVE('',#821,#822,#506,.T.);
#975=EDGE_CURVE('',#822,#823,#507,.T.);
#976=EDGE_CURVE('',#817,#823,#508,.T.);
#977=EDGE_CURVE('',#813,#824,#509,.T.);
#978=EDGE_CURVE('',#824,#820,#510,.T.);
#979=EDGE_CURVE('',#822,#825,#511,.T.);
#980=EDGE_CURVE('',#825,#826,#512,.T.);
#981=EDGE_CURVE('',#823,#826,#513,.T.);
#982=EDGE_CURVE('',#827,#821,#514,.T.);
#983=EDGE_CURVE('',#827,#824,#515,.T.);
#984=EDGE_CURVE('',#826,#816,#516,.T.);
#985=EDGE_CURVE('',#825,#827,#517,.T.);
#986=EDGE_CURVE('',#828,#829,#518,.T.);
#987=EDGE_CURVE('',#830,#828,#519,.T.);
#988=EDGE_CURVE('',#831,#830,#520,.T.);
#989=EDGE_CURVE('',#829,#831,#521,.T.);
#990=EDGE_CURVE('',#832,#833,#522,.T.);
#991=EDGE_CURVE('',#834,#832,#523,.T.);
#992=EDGE_CURVE('',#835,#834,#524,.T.);
#993=EDGE_CURVE('',#833,#835,#525,.T.);
#994=EDGE_CURVE('',#831,#834,#526,.T.);
#995=EDGE_CURVE('',#835,#830,#527,.T.);
#996=EDGE_CURVE('',#836,#828,#528,.T.);
#997=EDGE_CURVE('',#837,#836,#529,.T.);
#998=EDGE_CURVE('',#837,#838,#530,.T.);
#999=EDGE_CURVE('',#838,#839,#531,.T.);
#1000=EDGE_CURVE('',#833,#839,#532,.T.);
#1001=EDGE_CURVE('',#829,#840,#533,.T.);
#1002=EDGE_CURVE('',#840,#836,#534,.T.);
#1003=EDGE_CURVE('',#838,#841,#535,.T.);
#1004=EDGE_CURVE('',#841,#842,#536,.T.);
#1005=EDGE_CURVE('',#839,#842,#537,.T.);
#1006=EDGE_CURVE('',#843,#837,#538,.T.);
#1007=EDGE_CURVE('',#843,#840,#539,.T.);
#1008=EDGE_CURVE('',#842,#832,#540,.T.);
#1009=EDGE_CURVE('',#841,#843,#541,.T.);
#1010=EDGE_CURVE('',#844,#845,#542,.T.);
#1011=EDGE_CURVE('',#845,#846,#543,.T.);
#1012=EDGE_CURVE('',#847,#846,#544,.T.);
#1013=EDGE_CURVE('',#844,#847,#545,.T.);
#1014=EDGE_CURVE('',#848,#844,#546,.T.);
#1015=EDGE_CURVE('',#849,#847,#547,.T.);
#1016=EDGE_CURVE('',#848,#849,#548,.T.);
#1017=EDGE_CURVE('',#850,#848,#549,.T.);
#1018=EDGE_CURVE('',#851,#849,#550,.T.);
#1019=EDGE_CURVE('',#850,#851,#551,.T.);
#1020=EDGE_CURVE('',#845,#850,#552,.T.);
#1021=EDGE_CURVE('',#846,#851,#553,.T.);
#1022=EDGE_CURVE('',#852,#853,#554,.T.);
#1023=EDGE_CURVE('',#853,#854,#555,.T.);
#1024=EDGE_CURVE('',#855,#854,#556,.T.);
#1025=EDGE_CURVE('',#852,#855,#557,.T.);
#1026=EDGE_CURVE('',#856,#852,#558,.T.);
#1027=EDGE_CURVE('',#857,#855,#559,.T.);
#1028=EDGE_CURVE('',#856,#857,#560,.T.);
#1029=EDGE_CURVE('',#858,#856,#561,.T.);
#1030=EDGE_CURVE('',#859,#857,#562,.T.);
#1031=EDGE_CURVE('',#858,#859,#563,.T.);
#1032=EDGE_CURVE('',#853,#858,#564,.T.);
#1033=EDGE_CURVE('',#854,#859,#565,.T.);
#1034=EDGE_CURVE('',#860,#860,#740,.T.);
#1035=EDGE_CURVE('',#860,#861,#566,.T.);
#1036=EDGE_CURVE('',#861,#861,#741,.T.);
#1037=EDGE_CURVE('',#862,#862,#742,.T.);
#1038=EDGE_CURVE('',#862,#863,#567,.T.);
#1039=EDGE_CURVE('',#863,#863,#743,.T.);
#1040=EDGE_CURVE('',#864,#864,#744,.T.);
#1041=EDGE_CURVE('',#864,#865,#568,.T.);
#1042=EDGE_CURVE('',#865,#865,#745,.T.);
#1043=EDGE_CURVE('',#866,#866,#746,.T.);
#1044=EDGE_CURVE('',#866,#867,#569,.T.);
#1045=EDGE_CURVE('',#867,#867,#747,.T.);
#1046=EDGE_CURVE('',#868,#868,#748,.T.);
#1047=EDGE_CURVE('',#868,#869,#570,.T.);
#1048=EDGE_CURVE('',#869,#869,#749,.T.);
#1049=EDGE_CURVE('',#870,#870,#750,.T.);
#1050=EDGE_CURVE('',#870,#871,#571,.T.);
#1051=EDGE_CURVE('',#871,#871,#751,.T.);
#1052=ORIENTED_EDGE('',*,*,#872,.F.);
#1053=ORIENTED_EDGE('',*,*,#873,.T.);
#1054=ORIENTED_EDGE('',*,*,#874,.T.);
#1055=ORIENTED_EDGE('',*,*,#873,.F.);
#1056=ORIENTED_EDGE('',*,*,#874,.F.);
#1057=ORIENTED_EDGE('',*,*,#875,.F.);
#1058=ORIENTED_EDGE('',*,*,#876,.T.);
#1059=ORIENTED_EDGE('',*,*,#877,.T.);
#1060=ORIENTED_EDGE('',*,*,#876,.F.);
#1061=ORIENTED_EDGE('',*,*,#877,.F.);
#1062=ORIENTED_EDGE('',*,*,#878,.F.);
#1063=ORIENTED_EDGE('',*,*,#879,.T.);
#1064=ORIENTED_EDGE('',*,*,#880,.T.);
#1065=ORIENTED_EDGE('',*,*,#879,.F.);
#1066=ORIENTED_EDGE('',*,*,#880,.F.);
#1067=ORIENTED_EDGE('',*,*,#881,.F.);
#1068=ORIENTED_EDGE('',*,*,#882,.T.);
#1069=ORIENTED_EDGE('',*,*,#883,.T.);
#1070=ORIENTED_EDGE('',*,*,#882,.F.);
#1071=ORIENTED_EDGE('',*,*,#883,.F.);
#1072=ORIENTED_EDGE('',*,*,#884,.F.);
#1073=ORIENTED_EDGE('',*,*,#885,.T.);
#1074=ORIENTED_EDGE('',*,*,#886,.T.);
#1075=ORIENTED_EDGE('',*,*,#885,.F.);
#1076=ORIENTED_EDGE('',*,*,#886,.F.);
#1077=ORIENTED_EDGE('',*,*,#887,.F.);
#1078=ORIENTED_EDGE('',*,*,#888,.T.);
#1079=ORIENTED_EDGE('',*,*,#889,.T.);
#1080=ORIENTED_EDGE('',*,*,#888,.F.);
#1081=ORIENTED_EDGE('',*,*,#889,.F.);
#1082=ORIENTED_EDGE('',*,*,#890,.F.);
#1083=ORIENTED_EDGE('',*,*,#891,.F.);
#1084=ORIENTED_EDGE('',*,*,#892,.F.);
#1085=ORIENTED_EDGE('',*,*,#893,.F.);
#1086=ORIENTED_EDGE('',*,*,#894,.F.);
#1087=ORIENTED_EDGE('',*,*,#895,.F.);
#1088=ORIENTED_EDGE('',*,*,#896,.F.);
#1089=ORIENTED_EDGE('',*,*,#897,.F.);
#1090=ORIENTED_EDGE('',*,*,#898,.F.);
#1091=ORIENTED_EDGE('',*,*,#899,.F.);
#1092=ORIENTED_EDGE('',*,*,#900,.F.);
#1093=ORIENTED_EDGE('',*,*,#901,.T.);
#1094=ORIENTED_EDGE('',*,*,#902,.F.);
#1095=ORIENTED_EDGE('',*,*,#903,.F.);
#1096=ORIENTED_EDGE('',*,*,#904,.F.);
#1097=ORIENTED_EDGE('',*,*,#905,.T.);
#1098=ORIENTED_EDGE('',*,*,#906,.F.);
#1099=ORIENTED_EDGE('',*,*,#907,.F.);
#1100=ORIENTED_EDGE('',*,*,#908,.F.);
#1101=ORIENTED_EDGE('',*,*,#909,.F.);
#1102=ORIENTED_EDGE('',*,*,#910,.F.);
#1103=ORIENTED_EDGE('',*,*,#905,.F.);
#1104=ORIENTED_EDGE('',*,*,#911,.T.);
#1105=ORIENTED_EDGE('',*,*,#912,.F.);
#1106=ORIENTED_EDGE('',*,*,#913,.F.);
#1107=ORIENTED_EDGE('',*,*,#901,.F.);
#1108=ORIENTED_EDGE('',*,*,#914,.T.);
#1109=ORIENTED_EDGE('',*,*,#915,.F.);
#1110=ORIENTED_EDGE('',*,*,#916,.F.);
#1111=ORIENTED_EDGE('',*,*,#917,.F.);
#1112=ORIENTED_EDGE('',*,*,#918,.T.);
#1113=ORIENTED_EDGE('',*,*,#891,.T.);
#1114=ORIENTED_EDGE('',*,*,#919,.F.);
#1115=ORIENTED_EDGE('',*,*,#920,.F.);
#1116=ORIENTED_EDGE('',*,*,#921,.T.);
#1117=ORIENTED_EDGE('',*,*,#895,.T.);
#1118=ORIENTED_EDGE('',*,*,#902,.T.);
#1119=ORIENTED_EDGE('',*,*,#910,.T.);
#1120=ORIENTED_EDGE('',*,*,#922,.F.);
#1121=ORIENTED_EDGE('',*,*,#923,.F.);
#1122=ORIENTED_EDGE('',*,*,#894,.T.);
#1123=ORIENTED_EDGE('',*,*,#924,.F.);
#1124=ORIENTED_EDGE('',*,*,#925,.F.);
#1125=ORIENTED_EDGE('',*,*,#906,.T.);
#1126=ORIENTED_EDGE('',*,*,#903,.T.);
#1127=ORIENTED_EDGE('',*,*,#923,.T.);
#1128=ORIENTED_EDGE('',*,*,#926,.F.);
#1129=ORIENTED_EDGE('',*,*,#927,.T.);
#1130=ORIENTED_EDGE('',*,*,#887,.T.);
#1131=ORIENTED_EDGE('',*,*,#897,.T.);
#1132=ORIENTED_EDGE('',*,*,#928,.T.);
#1133=ORIENTED_EDGE('',*,*,#929,.T.);
#1134=ORIENTED_EDGE('',*,*,#924,.T.);
#1135=ORIENTED_EDGE('',*,*,#904,.T.);
#1136=ORIENTED_EDGE('',*,*,#927,.F.);
#1137=ORIENTED_EDGE('',*,*,#930,.F.);
#1138=ORIENTED_EDGE('',*,*,#911,.F.);
#1139=ORIENTED_EDGE('',*,*,#896,.T.);
#1140=ORIENTED_EDGE('',*,*,#921,.F.);
#1141=ORIENTED_EDGE('',*,*,#931,.F.);
#1142=ORIENTED_EDGE('',*,*,#928,.F.);
#1143=ORIENTED_EDGE('',*,*,#898,.T.);
#1144=ORIENTED_EDGE('',*,*,#913,.T.);
#1145=ORIENTED_EDGE('',*,*,#932,.F.);
#1146=ORIENTED_EDGE('',*,*,#933,.F.);
#1147=ORIENTED_EDGE('',*,*,#890,.T.);
#1148=ORIENTED_EDGE('',*,*,#934,.F.);
#1149=ORIENTED_EDGE('',*,*,#935,.F.);
#1150=ORIENTED_EDGE('',*,*,#919,.T.);
#1151=ORIENTED_EDGE('',*,*,#899,.T.);
#1152=ORIENTED_EDGE('',*,*,#933,.T.);
#1153=ORIENTED_EDGE('',*,*,#936,.F.);
#1154=ORIENTED_EDGE('',*,*,#937,.T.);
#1155=ORIENTED_EDGE('',*,*,#884,.T.);
#1156=ORIENTED_EDGE('',*,*,#893,.T.);
#1157=ORIENTED_EDGE('',*,*,#938,.T.);
#1158=ORIENTED_EDGE('',*,*,#939,.T.);
#1159=ORIENTED_EDGE('',*,*,#934,.T.);
#1160=ORIENTED_EDGE('',*,*,#900,.T.);
#1161=ORIENTED_EDGE('',*,*,#937,.F.);
#1162=ORIENTED_EDGE('',*,*,#940,.F.);
#1163=ORIENTED_EDGE('',*,*,#914,.F.);
#1164=ORIENTED_EDGE('',*,*,#892,.T.);
#1165=ORIENTED_EDGE('',*,*,#918,.F.);
#1166=ORIENTED_EDGE('',*,*,#941,.F.);
#1167=ORIENTED_EDGE('',*,*,#938,.F.);
#1168=ORIENTED_EDGE('',*,*,#931,.T.);
#1169=ORIENTED_EDGE('',*,*,#920,.T.);
#1170=ORIENTED_EDGE('',*,*,#935,.T.);
#1171=ORIENTED_EDGE('',*,*,#939,.F.);
#1172=ORIENTED_EDGE('',*,*,#941,.T.);
#1173=ORIENTED_EDGE('',*,*,#917,.T.);
#1174=ORIENTED_EDGE('',*,*,#942,.T.);
#1175=ORIENTED_EDGE('',*,*,#943,.T.);
#1176=ORIENTED_EDGE('',*,*,#944,.F.);
#1177=ORIENTED_EDGE('',*,*,#907,.T.);
#1178=ORIENTED_EDGE('',*,*,#925,.T.);
#1179=ORIENTED_EDGE('',*,*,#929,.F.);
#1180=ORIENTED_EDGE('',*,*,#916,.T.);
#1181=ORIENTED_EDGE('',*,*,#945,.F.);
#1182=ORIENTED_EDGE('',*,*,#946,.F.);
#1183=ORIENTED_EDGE('',*,*,#942,.F.);
#1184=ORIENTED_EDGE('',*,*,#930,.T.);
#1185=ORIENTED_EDGE('',*,*,#926,.T.);
#1186=ORIENTED_EDGE('',*,*,#922,.T.);
#1187=ORIENTED_EDGE('',*,*,#909,.T.);
#1188=ORIENTED_EDGE('',*,*,#947,.F.);
#1189=ORIENTED_EDGE('',*,*,#948,.F.);
#1190=ORIENTED_EDGE('',*,*,#945,.T.);
#1191=ORIENTED_EDGE('',*,*,#915,.T.);
#1192=ORIENTED_EDGE('',*,*,#940,.T.);
#1193=ORIENTED_EDGE('',*,*,#936,.T.);
#1194=ORIENTED_EDGE('',*,*,#932,.T.);
#1195=ORIENTED_EDGE('',*,*,#912,.T.);
#1196=ORIENTED_EDGE('',*,*,#946,.T.);
#1197=ORIENTED_EDGE('',*,*,#948,.T.);
#1198=ORIENTED_EDGE('',*,*,#949,.F.);
#1199=ORIENTED_EDGE('',*,*,#943,.F.);
#1200=ORIENTED_EDGE('',*,*,#872,.T.);
#1201=ORIENTED_EDGE('',*,*,#875,.T.);
#1202=ORIENTED_EDGE('',*,*,#878,.T.);
#1203=ORIENTED_EDGE('',*,*,#881,.T.);
#1204=ORIENTED_EDGE('',*,*,#908,.T.);
#1205=ORIENTED_EDGE('',*,*,#944,.T.);
#1206=ORIENTED_EDGE('',*,*,#949,.T.);
#1207=ORIENTED_EDGE('',*,*,#947,.T.);
#1208=ORIENTED_EDGE('',*,*,#950,.F.);
#1209=ORIENTED_EDGE('',*,*,#951,.T.);
#1210=ORIENTED_EDGE('',*,*,#952,.T.);
#1211=ORIENTED_EDGE('',*,*,#951,.F.);
#1212=ORIENTED_EDGE('',*,*,#952,.F.);
#1213=ORIENTED_EDGE('',*,*,#953,.F.);
#1214=ORIENTED_EDGE('',*,*,#954,.T.);
#1215=ORIENTED_EDGE('',*,*,#955,.T.);
#1216=ORIENTED_EDGE('',*,*,#954,.F.);
#1217=ORIENTED_EDGE('',*,*,#955,.F.);
#1218=ORIENTED_EDGE('',*,*,#956,.F.);
#1219=ORIENTED_EDGE('',*,*,#957,.T.);
#1220=ORIENTED_EDGE('',*,*,#958,.T.);
#1221=ORIENTED_EDGE('',*,*,#957,.F.);
#1222=ORIENTED_EDGE('',*,*,#958,.F.);
#1223=ORIENTED_EDGE('',*,*,#959,.F.);
#1224=ORIENTED_EDGE('',*,*,#960,.T.);
#1225=ORIENTED_EDGE('',*,*,#961,.T.);
#1226=ORIENTED_EDGE('',*,*,#960,.F.);
#1227=ORIENTED_EDGE('',*,*,#961,.F.);
#1228=ORIENTED_EDGE('',*,*,#962,.F.);
#1229=ORIENTED_EDGE('',*,*,#963,.F.);
#1230=ORIENTED_EDGE('',*,*,#964,.F.);
#1231=ORIENTED_EDGE('',*,*,#965,.F.);
#1232=ORIENTED_EDGE('',*,*,#966,.F.);
#1233=ORIENTED_EDGE('',*,*,#967,.F.);
#1234=ORIENTED_EDGE('',*,*,#968,.F.);
#1235=ORIENTED_EDGE('',*,*,#969,.F.);
#1236=ORIENTED_EDGE('',*,*,#970,.F.);
#1237=ORIENTED_EDGE('',*,*,#964,.T.);
#1238=ORIENTED_EDGE('',*,*,#971,.F.);
#1239=ORIENTED_EDGE('',*,*,#968,.T.);
#1240=ORIENTED_EDGE('',*,*,#969,.T.);
#1241=ORIENTED_EDGE('',*,*,#971,.T.);
#1242=ORIENTED_EDGE('',*,*,#963,.T.);
#1243=ORIENTED_EDGE('',*,*,#972,.F.);
#1244=ORIENTED_EDGE('',*,*,#973,.F.);
#1245=ORIENTED_EDGE('',*,*,#974,.T.);
#1246=ORIENTED_EDGE('',*,*,#975,.T.);
#1247=ORIENTED_EDGE('',*,*,#976,.F.);
#1248=ORIENTED_EDGE('',*,*,#962,.T.);
#1249=ORIENTED_EDGE('',*,*,#977,.T.);
#1250=ORIENTED_EDGE('',*,*,#978,.T.);
#1251=ORIENTED_EDGE('',*,*,#972,.T.);
#1252=ORIENTED_EDGE('',*,*,#979,.T.);
#1253=ORIENTED_EDGE('',*,*,#980,.T.);
#1254=ORIENTED_EDGE('',*,*,#981,.F.);
#1255=ORIENTED_EDGE('',*,*,#975,.F.);
#1256=ORIENTED_EDGE('',*,*,#982,.T.);
#1257=ORIENTED_EDGE('',*,*,#973,.T.);
#1258=ORIENTED_EDGE('',*,*,#978,.F.);
#1259=ORIENTED_EDGE('',*,*,#983,.F.);
#1260=ORIENTED_EDGE('',*,*,#967,.T.);
#1261=ORIENTED_EDGE('',*,*,#984,.F.);
#1262=ORIENTED_EDGE('',*,*,#980,.F.);
#1263=ORIENTED_EDGE('',*,*,#985,.T.);
#1264=ORIENTED_EDGE('',*,*,#983,.T.);
#1265=ORIENTED_EDGE('',*,*,#977,.F.);
#1266=ORIENTED_EDGE('',*,*,#965,.T.);
#1267=ORIENTED_EDGE('',*,*,#970,.T.);
#1268=ORIENTED_EDGE('',*,*,#966,.T.);
#1269=ORIENTED_EDGE('',*,*,#976,.T.);
#1270=ORIENTED_EDGE('',*,*,#981,.T.);
#1271=ORIENTED_EDGE('',*,*,#984,.T.);
#1272=ORIENTED_EDGE('',*,*,#985,.F.);
#1273=ORIENTED_EDGE('',*,*,#979,.F.);
#1274=ORIENTED_EDGE('',*,*,#974,.F.);
#1275=ORIENTED_EDGE('',*,*,#982,.F.);
#1276=ORIENTED_EDGE('',*,*,#950,.T.);
#1277=ORIENTED_EDGE('',*,*,#953,.T.);
#1278=ORIENTED_EDGE('',*,*,#956,.T.);
#1279=ORIENTED_EDGE('',*,*,#959,.T.);
#1280=ORIENTED_EDGE('',*,*,#986,.F.);
#1281=ORIENTED_EDGE('',*,*,#987,.F.);
#1282=ORIENTED_EDGE('',*,*,#988,.F.);
#1283=ORIENTED_EDGE('',*,*,#989,.F.);
#1284=ORIENTED_EDGE('',*,*,#990,.F.);
#1285=ORIENTED_EDGE('',*,*,#991,.F.);
#1286=ORIENTED_EDGE('',*,*,#992,.F.);
#1287=ORIENTED_EDGE('',*,*,#993,.F.);
#1288=ORIENTED_EDGE('',*,*,#994,.F.);
#1289=ORIENTED_EDGE('',*,*,#988,.T.);
#1290=ORIENTED_EDGE('',*,*,#995,.F.);
#1291=ORIENTED_EDGE('',*,*,#992,.T.);
#1292=ORIENTED_EDGE('',*,*,#993,.T.);
#1293=ORIENTED_EDGE('',*,*,#995,.T.);
#1294=ORIENTED_EDGE('',*,*,#987,.T.);
#1295=ORIENTED_EDGE('',*,*,#996,.F.);
#1296=ORIENTED_EDGE('',*,*,#997,.F.);
#1297=ORIENTED_EDGE('',*,*,#998,.T.);
#1298=ORIENTED_EDGE('',*,*,#999,.T.);
#1299=ORIENTED_EDGE('',*,*,#1000,.F.);
#1300=ORIENTED_EDGE('',*,*,#986,.T.);
#1301=ORIENTED_EDGE('',*,*,#1001,.T.);
#1302=ORIENTED_EDGE('',*,*,#1002,.T.);
#1303=ORIENTED_EDGE('',*,*,#996,.T.);
#1304=ORIENTED_EDGE('',*,*,#1003,.T.);
#1305=ORIENTED_EDGE('',*,*,#1004,.T.);
#1306=ORIENTED_EDGE('',*,*,#1005,.F.);
#1307=ORIENTED_EDGE('',*,*,#999,.F.);
#1308=ORIENTED_EDGE('',*,*,#1006,.T.);
#1309=ORIENTED_EDGE('',*,*,#997,.T.);
#1310=ORIENTED_EDGE('',*,*,#1002,.F.);
#1311=ORIENTED_EDGE('',*,*,#1007,.F.);
#1312=ORIENTED_EDGE('',*,*,#991,.T.);
#1313=ORIENTED_EDGE('',*,*,#1008,.F.);
#1314=ORIENTED_EDGE('',*,*,#1004,.F.);
#1315=ORIENTED_EDGE('',*,*,#1009,.T.);
#1316=ORIENTED_EDGE('',*,*,#1007,.T.);
#1317=ORIENTED_EDGE('',*,*,#1001,.F.);
#1318=ORIENTED_EDGE('',*,*,#989,.T.);
#1319=ORIENTED_EDGE('',*,*,#994,.T.);
#1320=ORIENTED_EDGE('',*,*,#990,.T.);
#1321=ORIENTED_EDGE('',*,*,#1000,.T.);
#1322=ORIENTED_EDGE('',*,*,#1005,.T.);
#1323=ORIENTED_EDGE('',*,*,#1008,.T.);
#1324=ORIENTED_EDGE('',*,*,#1009,.F.);
#1325=ORIENTED_EDGE('',*,*,#1003,.F.);
#1326=ORIENTED_EDGE('',*,*,#998,.F.);
#1327=ORIENTED_EDGE('',*,*,#1006,.F.);
#1328=ORIENTED_EDGE('',*,*,#1010,.T.);
#1329=ORIENTED_EDGE('',*,*,#1011,.T.);
#1330=ORIENTED_EDGE('',*,*,#1012,.F.);
#1331=ORIENTED_EDGE('',*,*,#1013,.F.);
#1332=ORIENTED_EDGE('',*,*,#1014,.T.);
#1333=ORIENTED_EDGE('',*,*,#1013,.T.);
#1334=ORIENTED_EDGE('',*,*,#1015,.F.);
#1335=ORIENTED_EDGE('',*,*,#1016,.F.);
#1336=ORIENTED_EDGE('',*,*,#1017,.T.);
#1337=ORIENTED_EDGE('',*,*,#1016,.T.);
#1338=ORIENTED_EDGE('',*,*,#1018,.F.);
#1339=ORIENTED_EDGE('',*,*,#1019,.F.);
#1340=ORIENTED_EDGE('',*,*,#1020,.T.);
#1341=ORIENTED_EDGE('',*,*,#1019,.T.);
#1342=ORIENTED_EDGE('',*,*,#1021,.F.);
#1343=ORIENTED_EDGE('',*,*,#1011,.F.);
#1344=ORIENTED_EDGE('',*,*,#1021,.T.);
#1345=ORIENTED_EDGE('',*,*,#1018,.T.);
#1346=ORIENTED_EDGE('',*,*,#1015,.T.);
#1347=ORIENTED_EDGE('',*,*,#1012,.T.);
#1348=ORIENTED_EDGE('',*,*,#1020,.F.);
#1349=ORIENTED_EDGE('',*,*,#1010,.F.);
#1350=ORIENTED_EDGE('',*,*,#1014,.F.);
#1351=ORIENTED_EDGE('',*,*,#1017,.F.);
#1352=ORIENTED_EDGE('',*,*,#1022,.T.);
#1353=ORIENTED_EDGE('',*,*,#1023,.T.);
#1354=ORIENTED_EDGE('',*,*,#1024,.F.);
#1355=ORIENTED_EDGE('',*,*,#1025,.F.);
#1356=ORIENTED_EDGE('',*,*,#1026,.T.);
#1357=ORIENTED_EDGE('',*,*,#1025,.T.);
#1358=ORIENTED_EDGE('',*,*,#1027,.F.);
#1359=ORIENTED_EDGE('',*,*,#1028,.F.);
#1360=ORIENTED_EDGE('',*,*,#1029,.T.);
#1361=ORIENTED_EDGE('',*,*,#1028,.T.);
#1362=ORIENTED_EDGE('',*,*,#1030,.F.);
#1363=ORIENTED_EDGE('',*,*,#1031,.F.);
#1364=ORIENTED_EDGE('',*,*,#1032,.T.);
#1365=ORIENTED_EDGE('',*,*,#1031,.T.);
#1366=ORIENTED_EDGE('',*,*,#1033,.F.);
#1367=ORIENTED_EDGE('',*,*,#1023,.F.);
#1368=ORIENTED_EDGE('',*,*,#1033,.T.);
#1369=ORIENTED_EDGE('',*,*,#1030,.T.);
#1370=ORIENTED_EDGE('',*,*,#1027,.T.);
#1371=ORIENTED_EDGE('',*,*,#1024,.T.);
#1372=ORIENTED_EDGE('',*,*,#1032,.F.);
#1373=ORIENTED_EDGE('',*,*,#1022,.F.);
#1374=ORIENTED_EDGE('',*,*,#1026,.F.);
#1375=ORIENTED_EDGE('',*,*,#1029,.F.);
#1376=ORIENTED_EDGE('',*,*,#1034,.F.);
#1377=ORIENTED_EDGE('',*,*,#1035,.T.);
#1378=ORIENTED_EDGE('',*,*,#1036,.F.);
#1379=ORIENTED_EDGE('',*,*,#1035,.F.);
#1380=ORIENTED_EDGE('',*,*,#1034,.T.);
#1381=ORIENTED_EDGE('',*,*,#1037,.F.);
#1382=ORIENTED_EDGE('',*,*,#1038,.T.);
#1383=ORIENTED_EDGE('',*,*,#1039,.T.);
#1384=ORIENTED_EDGE('',*,*,#1038,.F.);
#1385=ORIENTED_EDGE('',*,*,#1039,.F.);
#1386=ORIENTED_EDGE('',*,*,#1040,.F.);
#1387=ORIENTED_EDGE('',*,*,#1041,.T.);
#1388=ORIENTED_EDGE('',*,*,#1042,.T.);
#1389=ORIENTED_EDGE('',*,*,#1041,.F.);
#1390=ORIENTED_EDGE('',*,*,#1040,.T.);
#1391=ORIENTED_EDGE('',*,*,#1036,.T.);
#1392=ORIENTED_EDGE('',*,*,#1042,.F.);
#1393=ORIENTED_EDGE('',*,*,#1037,.T.);
#1394=ORIENTED_EDGE('',*,*,#1043,.F.);
#1395=ORIENTED_EDGE('',*,*,#1044,.T.);
#1396=ORIENTED_EDGE('',*,*,#1045,.F.);
#1397=ORIENTED_EDGE('',*,*,#1044,.F.);
#1398=ORIENTED_EDGE('',*,*,#1043,.T.);
#1399=ORIENTED_EDGE('',*,*,#1046,.F.);
#1400=ORIENTED_EDGE('',*,*,#1047,.T.);
#1401=ORIENTED_EDGE('',*,*,#1048,.T.);
#1402=ORIENTED_EDGE('',*,*,#1047,.F.);
#1403=ORIENTED_EDGE('',*,*,#1046,.T.);
#1404=ORIENTED_EDGE('',*,*,#1045,.T.);
#1405=ORIENTED_EDGE('',*,*,#1048,.F.);
#1406=ORIENTED_EDGE('',*,*,#1049,.F.);
#1407=ORIENTED_EDGE('',*,*,#1050,.T.);
#1408=ORIENTED_EDGE('',*,*,#1051,.T.);
#1409=ORIENTED_EDGE('',*,*,#1050,.F.);
#1410=ORIENTED_EDGE('',*,*,#1049,.T.);
#1411=ORIENTED_EDGE('',*,*,#1051,.F.);
#1412=CYLINDRICAL_SURFACE('',#1616,0.409999999999997);
#1413=CYLINDRICAL_SURFACE('',#1620,0.409999999999997);
#1414=CYLINDRICAL_SURFACE('',#1624,0.409999999999997);
#1415=CYLINDRICAL_SURFACE('',#1628,0.409999999999997);
#1416=CYLINDRICAL_SURFACE('',#1632,0.620000000000001);
#1417=CYLINDRICAL_SURFACE('',#1636,0.620000000000005);
#1418=CYLINDRICAL_SURFACE('',#1663,0.619999999999997);
#1419=CYLINDRICAL_SURFACE('',#1667,0.62);
#1420=CYLINDRICAL_SURFACE('',#1671,0.62);
#1421=CYLINDRICAL_SURFACE('',#1675,0.619999999999997);
#1422=CYLINDRICAL_SURFACE('',#1715,0.6);
#1423=CYLINDRICAL_SURFACE('',#1719,0.6);
#1424=CYLINDRICAL_SURFACE('',#1723,1.25);
#1425=CYLINDRICAL_SURFACE('',#1729,0.6);
#1426=CYLINDRICAL_SURFACE('',#1733,5.);
#1427=CYLINDRICAL_SURFACE('',#1739,0.4);
#1428=ADVANCED_FACE('',(#233),#1412,.F.);
#1429=ADVANCED_FACE('',(#234),#160,.F.);
#1430=ADVANCED_FACE('',(#235),#1413,.F.);
#1431=ADVANCED_FACE('',(#236),#161,.F.);
#1432=ADVANCED_FACE('',(#237),#1414,.F.);
#1433=ADVANCED_FACE('',(#238),#162,.F.);
#1434=ADVANCED_FACE('',(#239),#1415,.F.);
#1435=ADVANCED_FACE('',(#240),#163,.F.);
#1436=ADVANCED_FACE('',(#241),#1416,.F.);
#1437=ADVANCED_FACE('',(#242),#164,.T.);
#1438=ADVANCED_FACE('',(#243),#1417,.F.);
#1439=ADVANCED_FACE('',(#244),#165,.T.);
#1440=ADVANCED_FACE('',(#245),#166,.F.);
#1441=ADVANCED_FACE('',(#246),#167,.F.);
#1442=ADVANCED_FACE('',(#247),#168,.F.);
#1443=ADVANCED_FACE('',(#248),#169,.F.);
#1444=ADVANCED_FACE('',(#249),#170,.F.);
#1445=ADVANCED_FACE('',(#250),#171,.T.);
#1446=ADVANCED_FACE('',(#251),#172,.T.);
#1447=ADVANCED_FACE('',(#252,#147),#173,.T.);
#1448=ADVANCED_FACE('',(#253),#174,.T.);
#1449=ADVANCED_FACE('',(#254),#175,.F.);
#1450=ADVANCED_FACE('',(#255),#176,.F.);
#1451=ADVANCED_FACE('',(#256),#177,.T.);
#1452=ADVANCED_FACE('',(#257),#178,.T.);
#1453=ADVANCED_FACE('',(#258,#148),#179,.T.);
#1454=ADVANCED_FACE('',(#259),#180,.T.);
#1455=ADVANCED_FACE('',(#260),#181,.F.);
#1456=ADVANCED_FACE('',(#261),#182,.F.);
#1457=ADVANCED_FACE('',(#262),#183,.T.);
#1458=ADVANCED_FACE('',(#263),#184,.F.);
#1459=ADVANCED_FACE('',(#264),#185,.T.);
#1460=ADVANCED_FACE('',(#265,#149,#150,#151,#152),#186,.T.);
#1461=ADVANCED_FACE('',(#266),#187,.T.);
#1462=ADVANCED_FACE('',(#267),#1418,.F.);
#1463=ADVANCED_FACE('',(#268),#188,.F.);
#1464=ADVANCED_FACE('',(#269),#1419,.F.);
#1465=ADVANCED_FACE('',(#270),#189,.F.);
#1466=ADVANCED_FACE('',(#271),#1420,.F.);
#1467=ADVANCED_FACE('',(#272),#190,.F.);
#1468=ADVANCED_FACE('',(#273),#1421,.F.);
#1469=ADVANCED_FACE('',(#274),#191,.F.);
#1470=ADVANCED_FACE('',(#275),#192,.F.);
#1471=ADVANCED_FACE('',(#276),#193,.F.);
#1472=ADVANCED_FACE('',(#277),#194,.T.);
#1473=ADVANCED_FACE('',(#278),#195,.T.);
#1474=ADVANCED_FACE('',(#279),#196,.T.);
#1475=ADVANCED_FACE('',(#280),#197,.T.);
#1476=ADVANCED_FACE('',(#281),#198,.T.);
#1477=ADVANCED_FACE('',(#282),#199,.T.);
#1478=ADVANCED_FACE('',(#283),#200,.T.);
#1479=ADVANCED_FACE('',(#284,#153,#154,#155,#156),#201,.F.);
#1480=ADVANCED_FACE('',(#285),#202,.F.);
#1481=ADVANCED_FACE('',(#286),#203,.F.);
#1482=ADVANCED_FACE('',(#287),#204,.T.);
#1483=ADVANCED_FACE('',(#288),#205,.T.);
#1484=ADVANCED_FACE('',(#289),#206,.T.);
#1485=ADVANCED_FACE('',(#290),#207,.T.);
#1486=ADVANCED_FACE('',(#291),#208,.T.);
#1487=ADVANCED_FACE('',(#292),#209,.T.);
#1488=ADVANCED_FACE('',(#293),#210,.T.);
#1489=ADVANCED_FACE('',(#294),#211,.F.);
#1490=ADVANCED_FACE('',(#295),#212,.T.);
#1491=ADVANCED_FACE('',(#296),#213,.T.);
#1492=ADVANCED_FACE('',(#297),#214,.T.);
#1493=ADVANCED_FACE('',(#298),#215,.T.);
#1494=ADVANCED_FACE('',(#299),#216,.T.);
#1495=ADVANCED_FACE('',(#300),#217,.F.);
#1496=ADVANCED_FACE('',(#301),#218,.T.);
#1497=ADVANCED_FACE('',(#302),#219,.T.);
#1498=ADVANCED_FACE('',(#303),#220,.T.);
#1499=ADVANCED_FACE('',(#304),#221,.T.);
#1500=ADVANCED_FACE('',(#305),#222,.T.);
#1501=ADVANCED_FACE('',(#306),#223,.F.);
#1502=ADVANCED_FACE('',(#307),#1422,.T.);
#1503=ADVANCED_FACE('',(#308),#224,.T.);
#1504=ADVANCED_FACE('',(#309),#1423,.T.);
#1505=ADVANCED_FACE('',(#310),#225,.F.);
#1506=ADVANCED_FACE('',(#311),#1424,.T.);
#1507=ADVANCED_FACE('',(#312,#157),#226,.T.);
#1508=ADVANCED_FACE('',(#313,#158),#227,.F.);
#1509=ADVANCED_FACE('',(#314),#1425,.T.);
#1510=ADVANCED_FACE('',(#315),#228,.T.);
#1511=ADVANCED_FACE('',(#316),#1426,.T.);
#1512=ADVANCED_FACE('',(#317,#159),#229,.T.);
#1513=ADVANCED_FACE('',(#318),#230,.F.);
#1514=ADVANCED_FACE('',(#319),#1427,.T.);
#1515=ADVANCED_FACE('',(#320),#231,.T.);
#1516=ADVANCED_FACE('',(#321),#232,.F.);
#1517=CLOSED_SHELL('',(#1428,#1429,#1430,#1431,#1432,#1433,#1434,#1435,
#1436,#1437,#1438,#1439,#1440,#1441,#1442,#1443,#1444,#1445,#1446,#1447,
#1448,#1449,#1450,#1451,#1452,#1453,#1454,#1455,#1456,#1457,#1458,#1459,
#1460,#1461));
#1518=CLOSED_SHELL('',(#1462,#1463,#1464,#1465,#1466,#1467,#1468,#1469,
#1470,#1471,#1472,#1473,#1474,#1475,#1476,#1477,#1478,#1479));
#1519=CLOSED_SHELL('',(#1480,#1481,#1482,#1483,#1484,#1485,#1486,#1487,
#1488,#1489));
#1520=CLOSED_SHELL('',(#1490,#1491,#1492,#1493,#1494,#1495));
#1521=CLOSED_SHELL('',(#1496,#1497,#1498,#1499,#1500,#1501));
#1522=CLOSED_SHELL('',(#1502,#1503,#1504,#1505,#1506,#1507,#1508));
#1523=CLOSED_SHELL('',(#1509,#1510,#1511,#1512,#1513));
#1524=CLOSED_SHELL('',(#1514,#1515,#1516));
#1525=DERIVED_UNIT_ELEMENT(#1541,1.);
#1526=DERIVED_UNIT_ELEMENT(#2675,-3.);
#1527=DERIVED_UNIT_ELEMENT(#1541,1.);
#1528=DERIVED_UNIT_ELEMENT(#2675,-3.);
#1529=DERIVED_UNIT_ELEMENT(#1541,1.);
#1530=DERIVED_UNIT_ELEMENT(#2675,-3.);
#1531=DERIVED_UNIT_ELEMENT(#1541,1.);
#1532=DERIVED_UNIT_ELEMENT(#2675,-3.);
#1533=DERIVED_UNIT_ELEMENT(#1541,1.);
#1534=DERIVED_UNIT_ELEMENT(#2675,-3.);
#1535=DERIVED_UNIT_ELEMENT(#1541,1.);
#1536=DERIVED_UNIT_ELEMENT(#2675,-3.);
#1537=DERIVED_UNIT_ELEMENT(#1541,1.);
#1538=DERIVED_UNIT_ELEMENT(#2675,-3.);
#1539=DERIVED_UNIT_ELEMENT(#1541,1.);
#1540=DERIVED_UNIT_ELEMENT(#2675,-3.);
#1541=(
MASS_UNIT()
NAMED_UNIT(*)
SI_UNIT(.KILO.,.GRAM.)
);
#1542=DERIVED_UNIT((#1525,#1526));
#1543=DERIVED_UNIT((#1527,#1528));
#1544=DERIVED_UNIT((#1529,#1530));
#1545=DERIVED_UNIT((#1531,#1532));
#1546=DERIVED_UNIT((#1533,#1534));
#1547=DERIVED_UNIT((#1535,#1536));
#1548=DERIVED_UNIT((#1537,#1538));
#1549=DERIVED_UNIT((#1539,#1540));
#1550=MEASURE_REPRESENTATION_ITEM('density measure',
POSITIVE_RATIO_MEASURE(7850.),#1542);
#1551=MEASURE_REPRESENTATION_ITEM('density measure',
POSITIVE_RATIO_MEASURE(7850.),#1543);
#1552=MEASURE_REPRESENTATION_ITEM('density measure',
POSITIVE_RATIO_MEASURE(7850.),#1544);
#1553=MEASURE_REPRESENTATION_ITEM('density measure',
POSITIVE_RATIO_MEASURE(7850.),#1545);
#1554=MEASURE_REPRESENTATION_ITEM('density measure',
POSITIVE_RATIO_MEASURE(7850.),#1546);
#1555=MEASURE_REPRESENTATION_ITEM('density measure',
POSITIVE_RATIO_MEASURE(7850.),#1547);
#1556=MEASURE_REPRESENTATION_ITEM('density measure',
POSITIVE_RATIO_MEASURE(7850.),#1548);
#1557=MEASURE_REPRESENTATION_ITEM('density measure',
POSITIVE_RATIO_MEASURE(7850.),#1549);
#1558=PROPERTY_DEFINITION_REPRESENTATION(#1598,#1574);
#1559=PROPERTY_DEFINITION_REPRESENTATION(#1599,#1575);
#1560=PROPERTY_DEFINITION_REPRESENTATION(#1600,#1576);
#1561=PROPERTY_DEFINITION_REPRESENTATION(#1601,#1577);
#1562=PROPERTY_DEFINITION_REPRESENTATION(#1602,#1578);
#1563=PROPERTY_DEFINITION_REPRESENTATION(#1603,#1579);
#1564=PROPERTY_DEFINITION_REPRESENTATION(#1604,#1580);
#1565=PROPERTY_DEFINITION_REPRESENTATION(#1605,#1581);
#1566=PROPERTY_DEFINITION_REPRESENTATION(#1606,#1582);
#1567=PROPERTY_DEFINITION_REPRESENTATION(#1607,#1583);
#1568=PROPERTY_DEFINITION_REPRESENTATION(#1608,#1584);
#1569=PROPERTY_DEFINITION_REPRESENTATION(#1609,#1585);
#1570=PROPERTY_DEFINITION_REPRESENTATION(#1610,#1586);
#1571=PROPERTY_DEFINITION_REPRESENTATION(#1611,#1587);
#1572=PROPERTY_DEFINITION_REPRESENTATION(#1612,#1588);
#1573=PROPERTY_DEFINITION_REPRESENTATION(#1613,#1589);
#1574=REPRESENTATION('material name',(#1590),#2665);
#1575=REPRESENTATION('density',(#1550),#2665);
#1576=REPRESENTATION('material name',(#1591),#2666);
#1577=REPRESENTATION('density',(#1551),#2666);
#1578=REPRESENTATION('material name',(#1592),#2667);
#1579=REPRESENTATION('density',(#1552),#2667);
#1580=REPRESENTATION('material name',(#1593),#2668);
#1581=REPRESENTATION('density',(#1553),#2668);
#1582=REPRESENTATION('material name',(#1594),#2669);
#1583=REPRESENTATION('density',(#1554),#2669);
#1584=REPRESENTATION('material name',(#1595),#2670);
#1585=REPRESENTATION('density',(#1555),#2670);
#1586=REPRESENTATION('material name',(#1596),#2671);
#1587=REPRESENTATION('density',(#1556),#2671);
#1588=REPRESENTATION('material name',(#1597),#2672);
#1589=REPRESENTATION('density',(#1557),#2672);
#1590=DESCRIPTIVE_REPRESENTATION_ITEM('Steel','Steel');
#1591=DESCRIPTIVE_REPRESENTATION_ITEM('Steel','Steel');
#1592=DESCRIPTIVE_REPRESENTATION_ITEM('Steel','Steel');
#1593=DESCRIPTIVE_REPRESENTATION_ITEM('Steel','Steel');
#1594=DESCRIPTIVE_REPRESENTATION_ITEM('Steel','Steel');
#1595=DESCRIPTIVE_REPRESENTATION_ITEM('Steel','Steel');
#1596=DESCRIPTIVE_REPRESENTATION_ITEM('Steel','Steel');
#1597=DESCRIPTIVE_REPRESENTATION_ITEM('Steel','Steel');
#1598=PROPERTY_DEFINITION('material property','material name',#2733);
#1599=PROPERTY_DEFINITION('material property','density of part',#2733);
#1600=PROPERTY_DEFINITION('material property','material name',#2734);
#1601=PROPERTY_DEFINITION('material property','density of part',#2734);
#1602=PROPERTY_DEFINITION('material property','material name',#2735);
#1603=PROPERTY_DEFINITION('material property','density of part',#2735);
#1604=PROPERTY_DEFINITION('material property','material name',#2736);
#1605=PROPERTY_DEFINITION('material property','density of part',#2736);
#1606=PROPERTY_DEFINITION('material property','material name',#2737);
#1607=PROPERTY_DEFINITION('material property','density of part',#2737);
#1608=PROPERTY_DEFINITION('material property','material name',#2738);
#1609=PROPERTY_DEFINITION('material property','density of part',#2738);
#1610=PROPERTY_DEFINITION('material property','material name',#2739);
#1611=PROPERTY_DEFINITION('material property','density of part',#2739);
#1612=PROPERTY_DEFINITION('material property','material name',#2740);
#1613=PROPERTY_DEFINITION('material property','density of part',#2740);
#1614=AXIS2_PLACEMENT_3D('',#2230,#1770,#1771);
#1615=AXIS2_PLACEMENT_3D('',#2231,#1772,#1773);
#1616=AXIS2_PLACEMENT_3D('',#2232,#1774,#1775);
#1617=AXIS2_PLACEMENT_3D('',#2234,#1776,#1777);
#1618=AXIS2_PLACEMENT_3D('',#2237,#1779,#1780);
#1619=AXIS2_PLACEMENT_3D('',#2238,#1781,#1782);
#1620=AXIS2_PLACEMENT_3D('',#2239,#1783,#1784);
#1621=AXIS2_PLACEMENT_3D('',#2241,#1785,#1786);
#1622=AXIS2_PLACEMENT_3D('',#2244,#1788,#1789);
#1623=AXIS2_PLACEMENT_3D('',#2245,#1790,#1791);
#1624=AXIS2_PLACEMENT_3D('',#2246,#1792,#1793);
#1625=AXIS2_PLACEMENT_3D('',#2248,#1794,#1795);
#1626=AXIS2_PLACEMENT_3D('',#2251,#1797,#1798);
#1627=AXIS2_PLACEMENT_3D('',#2252,#1799,#1800);
#1628=AXIS2_PLACEMENT_3D('',#2253,#1801,#1802);
#1629=AXIS2_PLACEMENT_3D('',#2255,#1803,#1804);
#1630=AXIS2_PLACEMENT_3D('',#2258,#1806,#1807);
#1631=AXIS2_PLACEMENT_3D('',#2259,#1808,#1809);
#1632=AXIS2_PLACEMENT_3D('',#2260,#1810,#1811);
#1633=AXIS2_PLACEMENT_3D('',#2262,#1812,#1813);
#1634=AXIS2_PLACEMENT_3D('',#2265,#1815,#1816);
#1635=AXIS2_PLACEMENT_3D('',#2266,#1817,#1818);
#1636=AXIS2_PLACEMENT_3D('',#2267,#1819,#1820);
#1637=AXIS2_PLACEMENT_3D('',#2269,#1821,#1822);
#1638=AXIS2_PLACEMENT_3D('',#2272,#1824,#1825);
#1639=AXIS2_PLACEMENT_3D('',#2273,#1826,#1827);
#1640=AXIS2_PLACEMENT_3D('',#2274,#1828,#1829);
#1641=AXIS2_PLACEMENT_3D('',#2283,#1834,#1835);
#1642=AXIS2_PLACEMENT_3D('',#2292,#1840,#1841);
#1643=AXIS2_PLACEMENT_3D('',#2301,#1846,#1847);
#1644=AXIS2_PLACEMENT_3D('',#2310,#1852,#1853);
#1645=AXIS2_PLACEMENT_3D('',#2339,#1870,#1871);
#1646=AXIS2_PLACEMENT_3D('',#2343,#1874,#1875);
#1647=AXIS2_PLACEMENT_3D('',#2347,#1878,#1879);
#1648=AXIS2_PLACEMENT_3D('',#2351,#1882,#1883);
#1649=AXIS2_PLACEMENT_3D('',#2355,#1886,#1887);
#1650=AXIS2_PLACEMENT_3D('',#2357,#1889,#1890);
#1651=AXIS2_PLACEMENT_3D('',#2359,#1892,#1893);
#1652=AXIS2_PLACEMENT_3D('',#2363,#1896,#1897);
#1653=AXIS2_PLACEMENT_3D('',#2367,#1900,#1901);
#1654=AXIS2_PLACEMENT_3D('',#2371,#1904,#1905);
#1655=AXIS2_PLACEMENT_3D('',#2375,#1908,#1909);
#1656=AXIS2_PLACEMENT_3D('',#2377,#1911,#1912);
#1657=AXIS2_PLACEMENT_3D('',#2379,#1914,#1915);
#1658=AXIS2_PLACEMENT_3D('',#2385,#1919,#1920);
#1659=AXIS2_PLACEMENT_3D('',#2389,#1923,#1924);
#1660=AXIS2_PLACEMENT_3D('',#2393,#1927,#1928);
#1661=AXIS2_PLACEMENT_3D('',#2395,#1930,#1931);
#1662=AXIS2_PLACEMENT_3D('',#2396,#1932,#1933);
#1663=AXIS2_PLACEMENT_3D('',#2397,#1934,#1935);
#1664=AXIS2_PLACEMENT_3D('',#2399,#1936,#1937);
#1665=AXIS2_PLACEMENT_3D('',#2402,#1939,#1940);
#1666=AXIS2_PLACEMENT_3D('',#2403,#1941,#1942);
#1667=AXIS2_PLACEMENT_3D('',#2404,#1943,#1944);
#1668=AXIS2_PLACEMENT_3D('',#2406,#1945,#1946);
#1669=AXIS2_PLACEMENT_3D('',#2409,#1948,#1949);
#1670=AXIS2_PLACEMENT_3D('',#2410,#1950,#1951);
#1671=AXIS2_PLACEMENT_3D('',#2411,#1952,#1953);
#1672=AXIS2_PLACEMENT_3D('',#2413,#1954,#1955);
#1673=AXIS2_PLACEMENT_3D('',#2416,#1957,#1958);
#1674=AXIS2_PLACEMENT_3D('',#2417,#1959,#1960);
#1675=AXIS2_PLACEMENT_3D('',#2418,#1961,#1962);
#1676=AXIS2_PLACEMENT_3D('',#2420,#1963,#1964);
#1677=AXIS2_PLACEMENT_3D('',#2423,#1966,#1967);
#1678=AXIS2_PLACEMENT_3D('',#2424,#1968,#1969);
#1679=AXIS2_PLACEMENT_3D('',#2425,#1970,#1971);
#1680=AXIS2_PLACEMENT_3D('',#2434,#1976,#1977);
#1681=AXIS2_PLACEMENT_3D('',#2443,#1982,#1983);
#1682=AXIS2_PLACEMENT_3D('',#2446,#1986,#1987);
#1683=AXIS2_PLACEMENT_3D('',#2456,#1993,#1994);
#1684=AXIS2_PLACEMENT_3D('',#2460,#1997,#1998);
#1685=AXIS2_PLACEMENT_3D('',#2466,#2002,#2003);
#1686=AXIS2_PLACEMENT_3D('',#2470,#2006,#2007);
#1687=AXIS2_PLACEMENT_3D('',#2473,#2010,#2011);
#1688=AXIS2_PLACEMENT_3D('',#2474,#2012,#2013);
#1689=AXIS2_PLACEMENT_3D('',#2475,#2014,#2015);
#1690=AXIS2_PLACEMENT_3D('',#2476,#2016,#2017);
#1691=AXIS2_PLACEMENT_3D('',#2485,#2022,#2023);
#1692=AXIS2_PLACEMENT_3D('',#2494,#2028,#2029);
#1693=AXIS2_PLACEMENT_3D('',#2497,#2032,#2033);
#1694=AXIS2_PLACEMENT_3D('',#2507,#2039,#2040);
#1695=AXIS2_PLACEMENT_3D('',#2511,#2043,#2044);
#1696=AXIS2_PLACEMENT_3D('',#2517,#2048,#2049);
#1697=AXIS2_PLACEMENT_3D('',#2521,#2052,#2053);
#1698=AXIS2_PLACEMENT_3D('',#2524,#2056,#2057);
#1699=AXIS2_PLACEMENT_3D('',#2525,#2058,#2059);
#1700=AXIS2_PLACEMENT_3D('',#2526,#2060,#2061);
#1701=AXIS2_PLACEMENT_3D('',#2527,#2062,#2063);
#1702=AXIS2_PLACEMENT_3D('',#2536,#2068,#2069);
#1703=AXIS2_PLACEMENT_3D('',#2542,#2073,#2074);
#1704=AXIS2_PLACEMENT_3D('',#2548,#2078,#2079);
#1705=AXIS2_PLACEMENT_3D('',#2551,#2082,#2083);
#1706=AXIS2_PLACEMENT_3D('',#2552,#2084,#2085);
#1707=AXIS2_PLACEMENT_3D('',#2553,#2086,#2087);
#1708=AXIS2_PLACEMENT_3D('',#2554,#2088,#2089);
#1709=AXIS2_PLACEMENT_3D('',#2563,#2094,#2095);
#1710=AXIS2_PLACEMENT_3D('',#2569,#2099,#2100);
#1711=AXIS2_PLACEMENT_3D('',#2575,#2104,#2105);
#1712=AXIS2_PLACEMENT_3D('',#2578,#2108,#2109);
#1713=AXIS2_PLACEMENT_3D('',#2579,#2110,#2111);
#1714=AXIS2_PLACEMENT_3D('',#2580,#2112,#2113);
#1715=AXIS2_PLACEMENT_3D('',#2581,#2114,#2115);
#1716=AXIS2_PLACEMENT_3D('',#2583,#2116,#2117);
#1717=AXIS2_PLACEMENT_3D('',#2586,#2119,#2120);
#1718=AXIS2_PLACEMENT_3D('',#2587,#2121,#2122);
#1719=AXIS2_PLACEMENT_3D('',#2588,#2123,#2124);
#1720=AXIS2_PLACEMENT_3D('',#2590,#2125,#2126);
#1721=AXIS2_PLACEMENT_3D('',#2593,#2128,#2129);
#1722=AXIS2_PLACEMENT_3D('',#2594,#2130,#2131);
#1723=AXIS2_PLACEMENT_3D('',#2595,#2132,#2133);
#1724=AXIS2_PLACEMENT_3D('',#2597,#2134,#2135);
#1725=AXIS2_PLACEMENT_3D('',#2600,#2137,#2138);
#1726=AXIS2_PLACEMENT_3D('',#2601,#2139,#2140);
#1727=AXIS2_PLACEMENT_3D('',#2602,#2141,#2142);
#1728=AXIS2_PLACEMENT_3D('',#2603,#2143,#2144);
#1729=AXIS2_PLACEMENT_3D('',#2604,#2145,#2146);
#1730=AXIS2_PLACEMENT_3D('',#2606,#2147,#2148);
#1731=AXIS2_PLACEMENT_3D('',#2609,#2150,#2151);
#1732=AXIS2_PLACEMENT_3D('',#2610,#2152,#2153);
#1733=AXIS2_PLACEMENT_3D('',#2611,#2154,#2155);
#1734=AXIS2_PLACEMENT_3D('',#2613,#2156,#2157);
#1735=AXIS2_PLACEMENT_3D('',#2616,#2159,#2160);
#1736=AXIS2_PLACEMENT_3D('',#2617,#2161,#2162);
#1737=AXIS2_PLACEMENT_3D('',#2618,#2163,#2164);
#1738=AXIS2_PLACEMENT_3D('',#2619,#2165,#2166);
#1739=AXIS2_PLACEMENT_3D('',#2620,#2167,#2168);
#1740=AXIS2_PLACEMENT_3D('',#2622,#2169,#2170);
#1741=AXIS2_PLACEMENT_3D('',#2625,#2172,#2173);
#1742=AXIS2_PLACEMENT_3D('',#2626,#2174,#2175);
#1743=AXIS2_PLACEMENT_3D('',#2627,#2176,#2177);
#1744=AXIS2_PLACEMENT_3D('',#2628,#2178,#2179);
#1745=AXIS2_PLACEMENT_3D('',#2629,#2180,#2181);
#1746=AXIS2_PLACEMENT_3D('',#2630,#2182,#2183);
#1747=AXIS2_PLACEMENT_3D('',#2631,#2184,#2185);
#1748=AXIS2_PLACEMENT_3D('',#2632,#2186,#2187);
#1749=AXIS2_PLACEMENT_3D('',#2633,#2188,#2189);
#1750=AXIS2_PLACEMENT_3D('',#2634,#2190,#2191);
#1751=AXIS2_PLACEMENT_3D('',#2635,#2192,#2193);
#1752=AXIS2_PLACEMENT_3D('',#2636,#2194,#2195);
#1753=AXIS2_PLACEMENT_3D('',#2637,#2196,#2197);
#1754=AXIS2_PLACEMENT_3D('',#2638,#2198,#2199);
#1755=AXIS2_PLACEMENT_3D('',#2639,#2200,#2201);
#1756=AXIS2_PLACEMENT_3D('',#2640,#2202,#2203);
#1757=AXIS2_PLACEMENT_3D('',#2641,#2204,#2205);
#1758=AXIS2_PLACEMENT_3D('',#2642,#2206,#2207);
#1759=AXIS2_PLACEMENT_3D('',#2643,#2208,#2209);
#1760=AXIS2_PLACEMENT_3D('',#2644,#2210,#2211);
#1761=AXIS2_PLACEMENT_3D('',#2645,#2212,#2213);
#1762=AXIS2_PLACEMENT_3D('',#2646,#2214,#2215);
#1763=AXIS2_PLACEMENT_3D('',#2647,#2216,#2217);
#1764=AXIS2_PLACEMENT_3D('',#2648,#2218,#2219);
#1765=AXIS2_PLACEMENT_3D('',#2649,#2220,#2221);
#1766=AXIS2_PLACEMENT_3D('',#2650,#2222,#2223);
#1767=AXIS2_PLACEMENT_3D('',#2651,#2224,#2225);
#1768=AXIS2_PLACEMENT_3D('',#2652,#2226,#2227);
#1769=AXIS2_PLACEMENT_3D('',#2653,#2228,#2229);
#1770=DIRECTION('axis',(0.,0.,1.));
#1771=DIRECTION('refdir',(1.,0.,0.));
#1772=DIRECTION('axis',(0.,0.,1.));
#1773=DIRECTION('refdir',(1.,0.,0.));
#1774=DIRECTION('center_axis',(1.,0.,0.));
#1775=DIRECTION('ref_axis',(0.,0.,-1.));
#1776=DIRECTION('center_axis',(1.,0.,0.));
#1777=DIRECTION('ref_axis',(0.,0.,-1.));
#1778=DIRECTION('',(1.,0.,0.));
#1779=DIRECTION('center_axis',(1.,0.,0.));
#1780=DIRECTION('ref_axis',(0.,0.,-1.));
#1781=DIRECTION('center_axis',(1.,0.,0.));
#1782=DIRECTION('ref_axis',(0.,0.,-1.));
#1783=DIRECTION('center_axis',(1.,0.,0.));
#1784=DIRECTION('ref_axis',(0.,0.,-1.));
#1785=DIRECTION('center_axis',(1.,0.,0.));
#1786=DIRECTION('ref_axis',(0.,0.,-1.));
#1787=DIRECTION('',(1.,0.,0.));
#1788=DIRECTION('center_axis',(1.,0.,0.));
#1789=DIRECTION('ref_axis',(0.,0.,-1.));
#1790=DIRECTION('center_axis',(1.,0.,0.));
#1791=DIRECTION('ref_axis',(0.,0.,-1.));
#1792=DIRECTION('center_axis',(1.,0.,0.));
#1793=DIRECTION('ref_axis',(0.,0.,-1.));
#1794=DIRECTION('center_axis',(1.,0.,0.));
#1795=DIRECTION('ref_axis',(0.,0.,-1.));
#1796=DIRECTION('',(1.,0.,0.));
#1797=DIRECTION('center_axis',(1.,0.,0.));
#1798=DIRECTION('ref_axis',(0.,0.,-1.));
#1799=DIRECTION('center_axis',(1.,0.,0.));
#1800=DIRECTION('ref_axis',(0.,0.,-1.));
#1801=DIRECTION('center_axis',(1.,0.,0.));
#1802=DIRECTION('ref_axis',(0.,0.,-1.));
#1803=DIRECTION('center_axis',(1.,0.,0.));
#1804=DIRECTION('ref_axis',(0.,0.,-1.));
#1805=DIRECTION('',(1.,0.,0.));
#1806=DIRECTION('center_axis',(1.,0.,0.));
#1807=DIRECTION('ref_axis',(0.,0.,-1.));
#1808=DIRECTION('center_axis',(1.,0.,0.));
#1809=DIRECTION('ref_axis',(0.,0.,-1.));
#1810=DIRECTION('center_axis',(-1.,0.,0.));
#1811=DIRECTION('ref_axis',(0.,0.,-1.));
#1812=DIRECTION('center_axis',(-1.,0.,0.));
#1813=DIRECTION('ref_axis',(0.,0.,-1.));
#1814=DIRECTION('',(-1.,0.,0.));
#1815=DIRECTION('center_axis',(-1.,0.,0.));
#1816=DIRECTION('ref_axis',(0.,0.,-1.));
#1817=DIRECTION('center_axis',(1.,0.,0.));
#1818=DIRECTION('ref_axis',(0.,0.,-1.));
#1819=DIRECTION('center_axis',(-1.,0.,0.));
#1820=DIRECTION('ref_axis',(0.,0.,-1.));
#1821=DIRECTION('center_axis',(-1.,0.,0.));
#1822=DIRECTION('ref_axis',(0.,0.,-1.));
#1823=DIRECTION('',(-1.,0.,0.));
#1824=DIRECTION('center_axis',(-1.,0.,0.));
#1825=DIRECTION('ref_axis',(0.,0.,-1.));
#1826=DIRECTION('center_axis',(1.,0.,0.));
#1827=DIRECTION('ref_axis',(0.,0.,-1.));
#1828=DIRECTION('center_axis',(0.,1.,0.));
#1829=DIRECTION('ref_axis',(-1.,0.,0.));
#1830=DIRECTION('',(1.,0.,0.));
#1831=DIRECTION('',(0.,0.,1.));
#1832=DIRECTION('',(-1.,0.,0.));
#1833=DIRECTION('',(0.,0.,-1.));
#1834=DIRECTION('center_axis',(0.,1.,0.));
#1835=DIRECTION('ref_axis',(-1.,0.,0.));
#1836=DIRECTION('',(1.,0.,0.));
#1837=DIRECTION('',(0.,0.,1.));
#1838=DIRECTION('',(-1.,0.,0.));
#1839=DIRECTION('',(0.,0.,-1.));
#1840=DIRECTION('center_axis',(0.,-1.,0.));
#1841=DIRECTION('ref_axis',(1.,0.,0.));
#1842=DIRECTION('',(-1.,0.,0.));
#1843=DIRECTION('',(0.,0.,1.));
#1844=DIRECTION('',(1.,0.,0.));
#1845=DIRECTION('',(0.,0.,1.));
#1846=DIRECTION('center_axis',(0.,-1.,0.));
#1847=DIRECTION('ref_axis',(1.,0.,0.));
#1848=DIRECTION('',(-1.,0.,0.));
#1849=DIRECTION('',(0.,0.,1.));
#1850=DIRECTION('',(1.,0.,0.));
#1851=DIRECTION('',(0.,0.,1.));
#1852=DIRECTION('center_axis',(-1.,0.,0.));
#1853=DIRECTION('ref_axis',(0.,-1.,0.));
#1854=DIRECTION('',(0.,-1.,0.));
#1855=DIRECTION('',(0.,0.,-1.));
#1856=DIRECTION('',(0.,1.,0.));
#1857=DIRECTION('',(0.,0.,1.));
#1858=DIRECTION('',(0.,-1.,0.));
#1859=DIRECTION('',(0.,-1.,0.));
#1860=DIRECTION('',(0.,0.,1.));
#1861=DIRECTION('',(0.,-1.,0.));
#1862=DIRECTION('',(0.,-1.,0.));
#1863=DIRECTION('',(0.,0.,1.));
#1864=DIRECTION('',(0.,-1.,0.));
#1865=DIRECTION('',(0.,0.,-1.));
#1866=DIRECTION('',(0.,-1.,0.));
#1867=DIRECTION('',(0.,-1.,0.));
#1868=DIRECTION('',(0.,0.,-1.));
#1869=DIRECTION('',(0.,-1.,0.));
#1870=DIRECTION('center_axis',(0.,0.,1.));
#1871=DIRECTION('ref_axis',(1.,0.,0.));
#1872=DIRECTION('',(-1.,0.,0.));
#1873=DIRECTION('',(0.,-1.,0.));
#1874=DIRECTION('center_axis',(0.,0.,1.));
#1875=DIRECTION('ref_axis',(1.,0.,0.));
#1876=DIRECTION('',(0.,-1.,0.));
#1877=DIRECTION('',(1.,0.,0.));
#1878=DIRECTION('center_axis',(1.,0.,0.));
#1879=DIRECTION('ref_axis',(0.,1.,0.));
#1880=DIRECTION('',(0.,0.,1.));
#1881=DIRECTION('',(0.,1.,0.));
#1882=DIRECTION('center_axis',(1.,0.,0.));
#1883=DIRECTION('ref_axis',(0.,1.,0.));
#1884=DIRECTION('',(0.,1.,0.));
#1885=DIRECTION('',(0.,0.,1.));
#1886=DIRECTION('center_axis',(0.,0.,1.));
#1887=DIRECTION('ref_axis',(1.,0.,0.));
#1888=DIRECTION('',(1.,0.,0.));
#1889=DIRECTION('center_axis',(0.,0.,1.));
#1890=DIRECTION('ref_axis',(1.,0.,0.));
#1891=DIRECTION('',(-1.,0.,0.));
#1892=DIRECTION('center_axis',(0.,0.,1.));
#1893=DIRECTION('ref_axis',(1.,0.,0.));
#1894=DIRECTION('',(-1.,0.,0.));
#1895=DIRECTION('',(0.,-1.,0.));
#1896=DIRECTION('center_axis',(0.,0.,1.));
#1897=DIRECTION('ref_axis',(1.,0.,0.));
#1898=DIRECTION('',(0.,-1.,0.));
#1899=DIRECTION('',(1.,0.,0.));
#1900=DIRECTION('center_axis',(1.,0.,0.));
#1901=DIRECTION('ref_axis',(0.,1.,0.));
#1902=DIRECTION('',(0.,0.,1.));
#1903=DIRECTION('',(0.,1.,0.));
#1904=DIRECTION('center_axis',(1.,0.,0.));
#1905=DIRECTION('ref_axis',(0.,1.,0.));
#1906=DIRECTION('',(0.,1.,0.));
#1907=DIRECTION('',(0.,0.,1.));
#1908=DIRECTION('center_axis',(0.,0.,1.));
#1909=DIRECTION('ref_axis',(1.,0.,0.));
#1910=DIRECTION('',(1.,0.,0.));
#1911=DIRECTION('center_axis',(0.,0.,1.));
#1912=DIRECTION('ref_axis',(1.,0.,0.));
#1913=DIRECTION('',(-1.,0.,0.));
#1914=DIRECTION('center_axis',(0.,1.,0.));
#1915=DIRECTION('ref_axis',(-1.,0.,0.));
#1916=DIRECTION('',(-1.,0.,0.));
#1917=DIRECTION('',(0.,0.,1.));
#1918=DIRECTION('',(-1.,0.,0.));
#1919=DIRECTION('center_axis',(0.,0.,1.));
#1920=DIRECTION('ref_axis',(1.,0.,0.));
#1921=DIRECTION('',(1.,0.,0.));
#1922=DIRECTION('',(0.,-1.,0.));
#1923=DIRECTION('center_axis',(0.,-1.,0.));
#1924=DIRECTION('ref_axis',(1.,0.,0.));
#1925=DIRECTION('',(1.,0.,0.));
#1926=DIRECTION('',(0.,0.,1.));
#1927=DIRECTION('center_axis',(-1.,0.,0.));
#1928=DIRECTION('ref_axis',(0.,-1.,0.));
#1929=DIRECTION('',(0.,-1.,0.));
#1930=DIRECTION('center_axis',(0.,0.,1.));
#1931=DIRECTION('ref_axis',(1.,0.,0.));
#1932=DIRECTION('axis',(0.,0.,1.));
#1933=DIRECTION('refdir',(1.,0.,0.));
#1934=DIRECTION('center_axis',(0.,0.,1.));
#1935=DIRECTION('ref_axis',(1.,0.,0.));
#1936=DIRECTION('center_axis',(0.,0.,1.));
#1937=DIRECTION('ref_axis',(1.,0.,0.));
#1938=DIRECTION('',(0.,0.,1.));
#1939=DIRECTION('center_axis',(0.,0.,1.));
#1940=DIRECTION('ref_axis',(1.,0.,0.));
#1941=DIRECTION('center_axis',(0.,0.,1.));
#1942=DIRECTION('ref_axis',(1.,0.,0.));
#1943=DIRECTION('center_axis',(0.,0.,1.));
#1944=DIRECTION('ref_axis',(1.,0.,0.));
#1945=DIRECTION('center_axis',(0.,0.,1.));
#1946=DIRECTION('ref_axis',(1.,0.,0.));
#1947=DIRECTION('',(0.,0.,1.));
#1948=DIRECTION('center_axis',(0.,0.,1.));
#1949=DIRECTION('ref_axis',(1.,0.,0.));
#1950=DIRECTION('center_axis',(0.,0.,1.));
#1951=DIRECTION('ref_axis',(1.,0.,0.));
#1952=DIRECTION('center_axis',(0.,0.,1.));
#1953=DIRECTION('ref_axis',(1.,0.,0.));
#1954=DIRECTION('center_axis',(0.,0.,1.));
#1955=DIRECTION('ref_axis',(1.,0.,0.));
#1956=DIRECTION('',(0.,0.,1.));
#1957=DIRECTION('center_axis',(0.,0.,1.));
#1958=DIRECTION('ref_axis',(1.,0.,0.));
#1959=DIRECTION('center_axis',(0.,0.,1.));
#1960=DIRECTION('ref_axis',(1.,0.,0.));
#1961=DIRECTION('center_axis',(0.,0.,1.));
#1962=DIRECTION('ref_axis',(1.,0.,0.));
#1963=DIRECTION('center_axis',(0.,0.,1.));
#1964=DIRECTION('ref_axis',(1.,0.,0.));
#1965=DIRECTION('',(0.,0.,1.));
#1966=DIRECTION('center_axis',(0.,0.,1.));
#1967=DIRECTION('ref_axis',(1.,0.,0.));
#1968=DIRECTION('center_axis',(0.,0.,1.));
#1969=DIRECTION('ref_axis',(1.,0.,0.));
#1970=DIRECTION('center_axis',(0.,-1.,0.));
#1971=DIRECTION('ref_axis',(1.,0.,0.));
#1972=DIRECTION('',(-1.,0.,0.));
#1973=DIRECTION('',(0.,0.,1.));
#1974=DIRECTION('',(1.,0.,0.));
#1975=DIRECTION('',(0.,0.,-1.));
#1976=DIRECTION('center_axis',(0.,1.,0.));
#1977=DIRECTION('ref_axis',(-1.,0.,0.));
#1978=DIRECTION('',(1.,0.,0.));
#1979=DIRECTION('',(0.,0.,1.));
#1980=DIRECTION('',(-1.,0.,0.));
#1981=DIRECTION('',(0.,0.,-1.));
#1982=DIRECTION('center_axis',(0.,0.,1.));
#1983=DIRECTION('ref_axis',(1.,0.,0.));
#1984=DIRECTION('',(0.,1.,0.));
#1985=DIRECTION('',(0.,-1.,0.));
#1986=DIRECTION('center_axis',(1.,0.,0.));
#1987=DIRECTION('ref_axis',(0.,1.,0.));
#1988=DIRECTION('',(0.,1.,0.));
#1989=DIRECTION('',(0.,0.,1.));
#1990=DIRECTION('',(0.,1.,0.));
#1991=DIRECTION('',(0.,0.,1.));
#1992=DIRECTION('',(0.,1.,0.));
#1993=DIRECTION('center_axis',(0.,0.,1.));
#1994=DIRECTION('ref_axis',(1.,0.,0.));
#1995=DIRECTION('',(0.,-1.,0.));
#1996=DIRECTION('',(1.,0.,0.));
#1997=DIRECTION('center_axis',(0.,1.,0.));
#1998=DIRECTION('ref_axis',(-1.,0.,0.));
#1999=DIRECTION('',(-1.,0.,0.));
#2000=DIRECTION('',(0.,0.,1.));
#2001=DIRECTION('',(-1.,0.,0.));
#2002=DIRECTION('center_axis',(0.,-1.,0.));
#2003=DIRECTION('ref_axis',(1.,0.,0.));
#2004=DIRECTION('',(1.,0.,0.));
#2005=DIRECTION('',(0.,0.,1.));
#2006=DIRECTION('center_axis',(-1.,0.,0.));
#2007=DIRECTION('ref_axis',(0.,-1.,0.));
#2008=DIRECTION('',(0.,-1.,0.));
#2009=DIRECTION('',(0.,-1.,0.));
#2010=DIRECTION('center_axis',(0.,0.,1.));
#2011=DIRECTION('ref_axis',(1.,0.,0.));
#2012=DIRECTION('center_axis',(0.,0.,1.));
#2013=DIRECTION('ref_axis',(1.,0.,0.));
#2014=DIRECTION('axis',(0.,0.,1.));
#2015=DIRECTION('refdir',(1.,0.,0.));
#2016=DIRECTION('center_axis',(0.,-1.,0.));
#2017=DIRECTION('ref_axis',(1.,0.,0.));
#2018=DIRECTION('',(-1.,0.,0.));
#2019=DIRECTION('',(0.,0.,1.));
#2020=DIRECTION('',(1.,0.,0.));
#2021=DIRECTION('',(0.,0.,-1.));
#2022=DIRECTION('center_axis',(0.,1.,0.));
#2023=DIRECTION('ref_axis',(-1.,0.,0.));
#2024=DIRECTION('',(1.,0.,0.));
#2025=DIRECTION('',(0.,0.,1.));
#2026=DIRECTION('',(-1.,0.,0.));
#2027=DIRECTION('',(0.,0.,-1.));
#2028=DIRECTION('center_axis',(0.,0.,1.));
#2029=DIRECTION('ref_axis',(1.,0.,0.));
#2030=DIRECTION('',(0.,1.,0.));
#2031=DIRECTION('',(0.,-1.,0.));
#2032=DIRECTION('center_axis',(1.,0.,0.));
#2033=DIRECTION('ref_axis',(0.,1.,0.));
#2034=DIRECTION('',(0.,1.,0.));
#2035=DIRECTION('',(0.,0.,1.));
#2036=DIRECTION('',(0.,1.,0.));
#2037=DIRECTION('',(0.,0.,1.));
#2038=DIRECTION('',(0.,1.,0.));
#2039=DIRECTION('center_axis',(0.,0.,1.));
#2040=DIRECTION('ref_axis',(1.,0.,0.));
#2041=DIRECTION('',(0.,-1.,0.));
#2042=DIRECTION('',(1.,0.,0.));
#2043=DIRECTION('center_axis',(0.,1.,0.));
#2044=DIRECTION('ref_axis',(-1.,0.,0.));
#2045=DIRECTION('',(-1.,0.,0.));
#2046=DIRECTION('',(0.,0.,1.));
#2047=DIRECTION('',(-1.,0.,0.));
#2048=DIRECTION('center_axis',(0.,-1.,0.));
#2049=DIRECTION('ref_axis',(1.,0.,0.));
#2050=DIRECTION('',(1.,0.,0.));
#2051=DIRECTION('',(0.,0.,1.));
#2052=DIRECTION('center_axis',(-1.,0.,0.));
#2053=DIRECTION('ref_axis',(0.,-1.,0.));
#2054=DIRECTION('',(0.,-1.,0.));
#2055=DIRECTION('',(0.,-1.,0.));
#2056=DIRECTION('center_axis',(0.,0.,1.));
#2057=DIRECTION('ref_axis',(1.,0.,0.));
#2058=DIRECTION('center_axis',(0.,0.,1.));
#2059=DIRECTION('ref_axis',(1.,0.,0.));
#2060=DIRECTION('axis',(0.,0.,1.));
#2061=DIRECTION('refdir',(1.,0.,0.));
#2062=DIRECTION('center_axis',(0.,1.,0.));
#2063=DIRECTION('ref_axis',(-1.,0.,0.));
#2064=DIRECTION('',(-1.,0.,0.));
#2065=DIRECTION('',(0.,0.,1.));
#2066=DIRECTION('',(-1.,0.,0.));
#2067=DIRECTION('',(0.,0.,1.));
#2068=DIRECTION('center_axis',(1.,0.,0.));
#2069=DIRECTION('ref_axis',(0.,1.,0.));
#2070=DIRECTION('',(0.,1.,0.));
#2071=DIRECTION('',(0.,1.,0.));
#2072=DIRECTION('',(0.,0.,1.));
#2073=DIRECTION('center_axis',(0.,-1.,0.));
#2074=DIRECTION('ref_axis',(1.,0.,0.));
#2075=DIRECTION('',(1.,0.,0.));
#2076=DIRECTION('',(1.,0.,0.));
#2077=DIRECTION('',(0.,0.,1.));
#2078=DIRECTION('center_axis',(-1.,0.,0.));
#2079=DIRECTION('ref_axis',(0.,-1.,0.));
#2080=DIRECTION('',(0.,-1.,0.));
#2081=DIRECTION('',(0.,-1.,0.));
#2082=DIRECTION('center_axis',(0.,0.,1.));
#2083=DIRECTION('ref_axis',(1.,0.,0.));
#2084=DIRECTION('center_axis',(0.,0.,1.));
#2085=DIRECTION('ref_axis',(1.,0.,0.));
#2086=DIRECTION('axis',(0.,0.,1.));
#2087=DIRECTION('refdir',(1.,0.,0.));
#2088=DIRECTION('center_axis',(0.,1.,0.));
#2089=DIRECTION('ref_axis',(-1.,0.,0.));
#2090=DIRECTION('',(-1.,0.,0.));
#2091=DIRECTION('',(0.,0.,1.));
#2092=DIRECTION('',(-1.,0.,0.));
#2093=DIRECTION('',(0.,0.,1.));
#2094=DIRECTION('center_axis',(1.,0.,0.));
#2095=DIRECTION('ref_axis',(0.,1.,0.));
#2096=DIRECTION('',(0.,1.,0.));
#2097=DIRECTION('',(0.,1.,0.));
#2098=DIRECTION('',(0.,0.,1.));
#2099=DIRECTION('center_axis',(0.,-1.,0.));
#2100=DIRECTION('ref_axis',(1.,0.,0.));
#2101=DIRECTION('',(1.,0.,0.));
#2102=DIRECTION('',(1.,0.,0.));
#2103=DIRECTION('',(0.,0.,1.));
#2104=DIRECTION('center_axis',(-1.,0.,0.));
#2105=DIRECTION('ref_axis',(0.,-1.,0.));
#2106=DIRECTION('',(0.,-1.,0.));
#2107=DIRECTION('',(0.,-1.,0.));
#2108=DIRECTION('center_axis',(0.,0.,1.));
#2109=DIRECTION('ref_axis',(1.,0.,0.));
#2110=DIRECTION('center_axis',(0.,0.,1.));
#2111=DIRECTION('ref_axis',(1.,0.,0.));
#2112=DIRECTION('axis',(0.,0.,1.));
#2113=DIRECTION('refdir',(1.,0.,0.));
#2114=DIRECTION('center_axis',(0.,0.,1.));
#2115=DIRECTION('ref_axis',(1.,0.,0.));
#2116=DIRECTION('center_axis',(0.,0.,1.));
#2117=DIRECTION('ref_axis',(1.,0.,0.));
#2118=DIRECTION('',(0.,0.,-1.));
#2119=DIRECTION('center_axis',(0.,0.,-1.));
#2120=DIRECTION('ref_axis',(1.,0.,0.));
#2121=DIRECTION('center_axis',(0.,0.,1.));
#2122=DIRECTION('ref_axis',(1.,0.,0.));
#2123=DIRECTION('center_axis',(0.,0.,1.));
#2124=DIRECTION('ref_axis',(1.,0.,0.));
#2125=DIRECTION('center_axis',(0.,0.,1.));
#2126=DIRECTION('ref_axis',(1.,0.,0.));
#2127=DIRECTION('',(0.,0.,-1.));
#2128=DIRECTION('center_axis',(0.,0.,1.));
#2129=DIRECTION('ref_axis',(1.,0.,0.));
#2130=DIRECTION('center_axis',(0.,0.,1.));
#2131=DIRECTION('ref_axis',(1.,0.,0.));
#2132=DIRECTION('center_axis',(0.,0.,1.));
#2133=DIRECTION('ref_axis',(1.,0.,0.));
#2134=DIRECTION('center_axis',(0.,0.,1.));
#2135=DIRECTION('ref_axis',(1.,0.,0.));
#2136=DIRECTION('',(0.,0.,-1.));
#2137=DIRECTION('center_axis',(0.,0.,1.));
#2138=DIRECTION('ref_axis',(1.,0.,0.));
#2139=DIRECTION('center_axis',(0.,0.,1.));
#2140=DIRECTION('ref_axis',(1.,0.,0.));
#2141=DIRECTION('center_axis',(0.,0.,1.));
#2142=DIRECTION('ref_axis',(1.,0.,0.));
#2143=DIRECTION('axis',(0.,0.,1.));
#2144=DIRECTION('refdir',(1.,0.,0.));
#2145=DIRECTION('center_axis',(0.,0.,1.));
#2146=DIRECTION('ref_axis',(1.,0.,0.));
#2147=DIRECTION('center_axis',(0.,0.,1.));
#2148=DIRECTION('ref_axis',(1.,0.,0.));
#2149=DIRECTION('',(0.,0.,-1.));
#2150=DIRECTION('center_axis',(0.,0.,-1.));
#2151=DIRECTION('ref_axis',(1.,0.,0.));
#2152=DIRECTION('center_axis',(0.,0.,1.));
#2153=DIRECTION('ref_axis',(1.,0.,0.));
#2154=DIRECTION('center_axis',(0.,0.,1.));
#2155=DIRECTION('ref_axis',(1.,0.,0.));
#2156=DIRECTION('center_axis',(0.,0.,1.));
#2157=DIRECTION('ref_axis',(1.,0.,0.));
#2158=DIRECTION('',(0.,0.,-1.));
#2159=DIRECTION('center_axis',(0.,0.,1.));
#2160=DIRECTION('ref_axis',(1.,0.,0.));
#2161=DIRECTION('center_axis',(0.,0.,1.));
#2162=DIRECTION('ref_axis',(1.,0.,0.));
#2163=DIRECTION('center_axis',(0.,0.,1.));
#2164=DIRECTION('ref_axis',(1.,0.,0.));
#2165=DIRECTION('axis',(0.,0.,1.));
#2166=DIRECTION('refdir',(1.,0.,0.));
#2167=DIRECTION('center_axis',(0.,0.,1.));
#2168=DIRECTION('ref_axis',(1.,0.,0.));
#2169=DIRECTION('center_axis',(0.,0.,1.));
#2170=DIRECTION('ref_axis',(1.,0.,0.));
#2171=DIRECTION('',(0.,0.,-1.));
#2172=DIRECTION('center_axis',(0.,0.,1.));
#2173=DIRECTION('ref_axis',(1.,0.,0.));
#2174=DIRECTION('center_axis',(0.,0.,1.));
#2175=DIRECTION('ref_axis',(1.,0.,0.));
#2176=DIRECTION('center_axis',(0.,0.,1.));
#2177=DIRECTION('ref_axis',(1.,0.,0.));
#2178=DIRECTION('',(0.,0.,1.));
#2179=DIRECTION('',(1.,0.,0.));
#2180=DIRECTION('',(0.,0.,1.));
#2181=DIRECTION('',(1.,0.,0.));
#2182=DIRECTION('',(1.22464679914735E-16,0.,-1.));
#2183=DIRECTION('',(-1.,0.,-1.22464679914735E-16));
#2184=DIRECTION('',(0.,0.,1.));
#2185=DIRECTION('',(1.,0.,0.));
#2186=DIRECTION('',(0.,0.,1.));
#2187=DIRECTION('',(1.,0.,0.));
#2188=DIRECTION('',(1.,0.,2.22044604925031E-16));
#2189=DIRECTION('',(2.22044604925031E-16,0.,-1.));
#2190=DIRECTION('',(0.,0.,1.));
#2191=DIRECTION('',(1.,0.,0.));
#2192=DIRECTION('',(1.,0.,2.22044604925031E-16));
#2193=DIRECTION('',(2.22044604925031E-16,0.,-1.));
#2194=DIRECTION('',(1.22464679914735E-16,0.,-1.));
#2195=DIRECTION('',(-1.,0.,-1.22464679914735E-16));
#2196=DIRECTION('',(0.,0.,1.));
#2197=DIRECTION('',(1.,0.,0.));
#2198=DIRECTION('',(0.,0.,1.));
#2199=DIRECTION('',(1.,0.,0.));
#2200=DIRECTION('',(0.,0.,1.));
#2201=DIRECTION('',(1.,0.,0.));
#2202=DIRECTION('',(0.,0.,1.));
#2203=DIRECTION('',(1.,0.,0.));
#2204=DIRECTION('',(1.22464679914735E-16,0.,-1.));
#2205=DIRECTION('',(-1.,0.,-1.22464679914735E-16));
#2206=DIRECTION('',(0.,0.,1.));
#2207=DIRECTION('',(1.,0.,0.));
#2208=DIRECTION('',(1.22464679914735E-16,0.,-1.));
#2209=DIRECTION('',(-1.,0.,-1.22464679914735E-16));
#2210=DIRECTION('',(0.,0.,1.));
#2211=DIRECTION('',(1.,0.,0.));
#2212=DIRECTION('',(0.,0.,1.));
#2213=DIRECTION('',(1.,0.,0.));
#2214=DIRECTION('',(1.,0.,2.22044604925031E-16));
#2215=DIRECTION('',(2.22044604925031E-16,0.,-1.));
#2216=DIRECTION('',(0.,0.,1.));
#2217=DIRECTION('',(1.,0.,0.));
#2218=DIRECTION('',(0.,0.,1.));
#2219=DIRECTION('',(1.,0.,0.));
#2220=DIRECTION('',(0.,0.,1.));
#2221=DIRECTION('',(1.,0.,0.));
#2222=DIRECTION('',(0.,0.,1.));
#2223=DIRECTION('',(1.,0.,0.));
#2224=DIRECTION('',(1.,0.,2.22044604925031E-16));
#2225=DIRECTION('',(2.22044604925031E-16,0.,-1.));
#2226=DIRECTION('',(1.,0.,2.22044604925031E-16));
#2227=DIRECTION('',(2.22044604925031E-16,0.,-1.));
#2228=DIRECTION('',(1.,0.,2.22044604925031E-16));
#2229=DIRECTION('',(2.22044604925031E-16,0.,-1.));
#2230=CARTESIAN_POINT('',(0.,0.,0.));
#2231=CARTESIAN_POINT('',(0.,0.,0.));
#2232=CARTESIAN_POINT('Origin',(0.,51.,56.7));
#2233=CARTESIAN_POINT('',(0.,51.,57.11));
#2234=CARTESIAN_POINT('Origin',(0.,51.,56.7));
#2235=CARTESIAN_POINT('',(1.5,51.,57.11));
#2236=CARTESIAN_POINT('',(0.,51.,57.11));
#2237=CARTESIAN_POINT('Origin',(1.5,51.,56.7));
#2238=CARTESIAN_POINT('Origin',(1.5,51.,56.7));
#2239=CARTESIAN_POINT('Origin',(0.,9.,113.3));
#2240=CARTESIAN_POINT('',(0.,9.,113.71));
#2241=CARTESIAN_POINT('Origin',(0.,9.,113.3));
#2242=CARTESIAN_POINT('',(1.5,9.,113.71));
#2243=CARTESIAN_POINT('',(0.,9.,113.71));
#2244=CARTESIAN_POINT('Origin',(1.5,9.,113.3));
#2245=CARTESIAN_POINT('Origin',(1.5,9.,113.3));
#2246=CARTESIAN_POINT('Origin',(0.,9.,56.7));
#2247=CARTESIAN_POINT('',(0.,9.,57.11));
#2248=CARTESIAN_POINT('Origin',(0.,9.,56.7));
#2249=CARTESIAN_POINT('',(1.5,9.,57.11));
#2250=CARTESIAN_POINT('',(0.,9.,57.11));
#2251=CARTESIAN_POINT('Origin',(1.5,9.,56.7));
#2252=CARTESIAN_POINT('Origin',(1.5,9.,56.7));
#2253=CARTESIAN_POINT('Origin',(0.,51.,113.3));
#2254=CARTESIAN_POINT('',(0.,51.,113.71));
#2255=CARTESIAN_POINT('Origin',(0.,51.,113.3));
#2256=CARTESIAN_POINT('',(1.5,51.,113.71));
#2257=CARTESIAN_POINT('',(0.,51.,113.71));
#2258=CARTESIAN_POINT('Origin',(1.5,51.,113.3));
#2259=CARTESIAN_POINT('Origin',(1.5,51.,113.3));
#2260=CARTESIAN_POINT('Origin',(1.8,30.,18.));
#2261=CARTESIAN_POINT('',(1.8,30.,18.62));
#2262=CARTESIAN_POINT('Origin',(1.8,30.,18.));
#2263=CARTESIAN_POINT('',(1.18,30.,18.62));
#2264=CARTESIAN_POINT('',(1.8,30.,18.62));
#2265=CARTESIAN_POINT('Origin',(1.18,30.,18.));
#2266=CARTESIAN_POINT('Origin',(1.18,30.,18.));
#2267=CARTESIAN_POINT('Origin',(1.8,30.,152.));
#2268=CARTESIAN_POINT('',(1.8,30.,152.62));
#2269=CARTESIAN_POINT('Origin',(1.8,30.,152.));
#2270=CARTESIAN_POINT('',(1.18,30.,152.62));
#2271=CARTESIAN_POINT('',(1.8,30.,152.62));
#2272=CARTESIAN_POINT('Origin',(1.18,30.,152.));
#2273=CARTESIAN_POINT('Origin',(1.18,30.,152.));
#2274=CARTESIAN_POINT('Origin',(1.81,58.82,0.));
#2275=CARTESIAN_POINT('',(1.3,58.82,84.08));
#2276=CARTESIAN_POINT('',(1.8,58.82,84.08));
#2277=CARTESIAN_POINT('',(1.6825,58.82,84.08));
#2278=CARTESIAN_POINT('',(1.3,58.82,1.82));
#2279=CARTESIAN_POINT('',(1.3,58.82,0.));
#2280=CARTESIAN_POINT('',(1.8,58.82,1.82));
#2281=CARTESIAN_POINT('',(1.6825,58.82,1.82));
#2282=CARTESIAN_POINT('',(1.8,58.82,0.));
#2283=CARTESIAN_POINT('Origin',(1.81,58.82,0.));
#2284=CARTESIAN_POINT('',(1.3,58.82,168.18));
#2285=CARTESIAN_POINT('',(1.8,58.82,168.18));
#2286=CARTESIAN_POINT('',(1.6825,58.82,168.18));
#2287=CARTESIAN_POINT('',(1.3,58.82,85.92));
#2288=CARTESIAN_POINT('',(1.3,58.82,0.));
#2289=CARTESIAN_POINT('',(1.8,58.82,85.92));
#2290=CARTESIAN_POINT('',(1.6825,58.82,85.92));
#2291=CARTESIAN_POINT('',(1.8,58.82,0.));
#2292=CARTESIAN_POINT('Origin',(1.3,58.18,0.));
#2293=CARTESIAN_POINT('',(1.8,58.18,84.08));
#2294=CARTESIAN_POINT('',(1.3,58.18,84.08));
#2295=CARTESIAN_POINT('',(1.4275,58.18,84.08));
#2296=CARTESIAN_POINT('',(1.8,58.18,1.82));
#2297=CARTESIAN_POINT('',(1.8,58.18,0.));
#2298=CARTESIAN_POINT('',(1.3,58.18,1.82));
#2299=CARTESIAN_POINT('',(1.4275,58.18,1.82));
#2300=CARTESIAN_POINT('',(1.3,58.18,0.));
#2301=CARTESIAN_POINT('Origin',(1.3,58.18,0.));
#2302=CARTESIAN_POINT('',(1.8,58.18,168.18));
#2303=CARTESIAN_POINT('',(1.3,58.18,168.18));
#2304=CARTESIAN_POINT('',(1.4275,58.18,168.18));
#2305=CARTESIAN_POINT('',(1.8,58.18,85.92));
#2306=CARTESIAN_POINT('',(1.8,58.18,0.));
#2307=CARTESIAN_POINT('',(1.3,58.18,85.92));
#2308=CARTESIAN_POINT('',(1.4275,58.18,85.92));
#2309=CARTESIAN_POINT('',(1.3,58.18,0.));
#2310=CARTESIAN_POINT('Origin',(1.3,60.,168.18));
#2311=CARTESIAN_POINT('',(1.3,60.,168.18));
#2312=CARTESIAN_POINT('',(1.3,60.,168.18));
#2313=CARTESIAN_POINT('',(1.3,60.,170.));
#2314=CARTESIAN_POINT('',(1.3,60.,84.09));
#2315=CARTESIAN_POINT('',(1.3,0.,170.));
#2316=CARTESIAN_POINT('',(1.3,45.,170.));
#2317=CARTESIAN_POINT('',(1.3,0.,168.18));
#2318=CARTESIAN_POINT('',(1.3,0.,84.09));
#2319=CARTESIAN_POINT('',(1.3,60.,168.18));
#2320=CARTESIAN_POINT('',(1.3,0.,85.92));
#2321=CARTESIAN_POINT('',(1.3,60.,85.92));
#2322=CARTESIAN_POINT('',(1.3,0.,84.08));
#2323=CARTESIAN_POINT('',(1.3,0.,42.04));
#2324=CARTESIAN_POINT('',(1.3,60.,84.08));
#2325=CARTESIAN_POINT('',(1.3,0.,1.82));
#2326=CARTESIAN_POINT('',(1.3,60.,1.82));
#2327=CARTESIAN_POINT('',(1.3,0.,0.));
#2328=CARTESIAN_POINT('',(1.3,0.,0.));
#2329=CARTESIAN_POINT('',(1.3,60.,0.));
#2330=CARTESIAN_POINT('',(1.3,45.,0.));
#2331=CARTESIAN_POINT('',(1.3,60.,1.82));
#2332=CARTESIAN_POINT('',(1.3,60.,0.));
#2333=CARTESIAN_POINT('',(1.3,60.,1.82));
#2334=CARTESIAN_POINT('',(1.3,60.,84.08));
#2335=CARTESIAN_POINT('',(1.3,60.,84.08));
#2336=CARTESIAN_POINT('',(1.3,60.,85.92));
#2337=CARTESIAN_POINT('',(1.3,60.,42.04));
#2338=CARTESIAN_POINT('',(1.3,60.,85.92));
#2339=CARTESIAN_POINT('Origin',(1.555,30.,168.18));
#2340=CARTESIAN_POINT('',(1.8,0.,168.18));
#2341=CARTESIAN_POINT('',(0.7775,0.,168.18));
#2342=CARTESIAN_POINT('',(1.8,15.,168.18));
#2343=CARTESIAN_POINT('Origin',(1.555,30.,168.18));
#2344=CARTESIAN_POINT('',(1.8,60.,168.18));
#2345=CARTESIAN_POINT('',(1.8,15.,168.18));
#2346=CARTESIAN_POINT('',(1.6775,60.,168.18));
#2347=CARTESIAN_POINT('Origin',(1.8,0.,0.));
#2348=CARTESIAN_POINT('',(1.8,0.,85.92));
#2349=CARTESIAN_POINT('',(1.8,0.,0.));
#2350=CARTESIAN_POINT('',(1.8,15.,85.92));
#2351=CARTESIAN_POINT('Origin',(1.8,0.,0.));
#2352=CARTESIAN_POINT('',(1.8,60.,85.92));
#2353=CARTESIAN_POINT('',(1.8,15.,85.92));
#2354=CARTESIAN_POINT('',(1.8,60.,0.));
#2355=CARTESIAN_POINT('Origin',(1.555,30.,85.92));
#2356=CARTESIAN_POINT('',(0.7775,0.,85.92));
#2357=CARTESIAN_POINT('Origin',(1.555,30.,85.92));
#2358=CARTESIAN_POINT('',(1.6775,60.,85.92));
#2359=CARTESIAN_POINT('Origin',(1.555,30.,84.08));
#2360=CARTESIAN_POINT('',(1.8,0.,84.08));
#2361=CARTESIAN_POINT('',(0.7775,0.,84.08));
#2362=CARTESIAN_POINT('',(1.8,15.,84.08));
#2363=CARTESIAN_POINT('Origin',(1.555,30.,84.08));
#2364=CARTESIAN_POINT('',(1.8,60.,84.08));
#2365=CARTESIAN_POINT('',(1.8,15.,84.08));
#2366=CARTESIAN_POINT('',(1.6775,60.,84.08));
#2367=CARTESIAN_POINT('Origin',(1.8,0.,0.));
#2368=CARTESIAN_POINT('',(1.8,0.,1.82));
#2369=CARTESIAN_POINT('',(1.8,0.,0.));
#2370=CARTESIAN_POINT('',(1.8,15.,1.82));
#2371=CARTESIAN_POINT('Origin',(1.8,0.,0.));
#2372=CARTESIAN_POINT('',(1.8,60.,1.82));
#2373=CARTESIAN_POINT('',(1.8,15.,1.82));
#2374=CARTESIAN_POINT('',(1.8,60.,0.));
#2375=CARTESIAN_POINT('Origin',(1.555,30.,1.82));
#2376=CARTESIAN_POINT('',(0.7775,0.,1.82));
#2377=CARTESIAN_POINT('Origin',(1.555,30.,1.82));
#2378=CARTESIAN_POINT('',(1.6775,60.,1.82));
#2379=CARTESIAN_POINT('Origin',(1.8,60.,0.));
#2380=CARTESIAN_POINT('',(0.,60.,0.));
#2381=CARTESIAN_POINT('',(1.8,60.,0.));
#2382=CARTESIAN_POINT('',(0.,60.,170.));
#2383=CARTESIAN_POINT('',(0.,60.,0.));
#2384=CARTESIAN_POINT('',(1.8,60.,170.));
#2385=CARTESIAN_POINT('Origin',(0.9,30.,0.));
#2386=CARTESIAN_POINT('',(0.,0.,0.));
#2387=CARTESIAN_POINT('',(0.,0.,0.));
#2388=CARTESIAN_POINT('',(0.,60.,0.));
#2389=CARTESIAN_POINT('Origin',(0.,0.,0.));
#2390=CARTESIAN_POINT('',(0.,0.,170.));
#2391=CARTESIAN_POINT('',(0.,0.,170.));
#2392=CARTESIAN_POINT('',(0.,0.,0.));
#2393=CARTESIAN_POINT('Origin',(0.,60.,0.));
#2394=CARTESIAN_POINT('',(0.,60.,170.));
#2395=CARTESIAN_POINT('Origin',(0.9,30.,170.));
#2396=CARTESIAN_POINT('',(0.,0.,0.));
#2397=CARTESIAN_POINT('Origin',(62.18,6.5,0.));
#2398=CARTESIAN_POINT('',(61.56,6.5,0.));
#2399=CARTESIAN_POINT('Origin',(62.18,6.5,0.));
#2400=CARTESIAN_POINT('',(61.56,6.5,1.2));
#2401=CARTESIAN_POINT('',(61.56,6.5,0.));
#2402=CARTESIAN_POINT('Origin',(62.18,6.5,1.2));
#2403=CARTESIAN_POINT('Origin',(62.18,6.5,1.2));
#2404=CARTESIAN_POINT('Origin',(5.18,53.5,0.));
#2405=CARTESIAN_POINT('',(4.56,53.5,0.));
#2406=CARTESIAN_POINT('Origin',(5.18,53.5,0.));
#2407=CARTESIAN_POINT('',(4.56,53.5,1.2));
#2408=CARTESIAN_POINT('',(4.56,53.5,0.));
#2409=CARTESIAN_POINT('Origin',(5.18,53.5,1.2));
#2410=CARTESIAN_POINT('Origin',(5.18,53.5,1.2));
#2411=CARTESIAN_POINT('Origin',(5.18,6.5,0.));
#2412=CARTESIAN_POINT('',(4.56,6.5,0.));
#2413=CARTESIAN_POINT('Origin',(5.18,6.5,0.));
#2414=CARTESIAN_POINT('',(4.56,6.5,1.2));
#2415=CARTESIAN_POINT('',(4.56,6.5,0.));
#2416=CARTESIAN_POINT('Origin',(5.18,6.5,1.2));
#2417=CARTESIAN_POINT('Origin',(5.18,6.5,1.2));
#2418=CARTESIAN_POINT('Origin',(62.18,53.5,0.));
#2419=CARTESIAN_POINT('',(61.56,53.5,0.));
#2420=CARTESIAN_POINT('Origin',(62.18,53.5,0.));
#2421=CARTESIAN_POINT('',(61.56,53.5,1.2));
#2422=CARTESIAN_POINT('',(61.56,53.5,0.));
#2423=CARTESIAN_POINT('Origin',(62.18,53.5,1.2));
#2424=CARTESIAN_POINT('Origin',(62.18,53.5,1.2));
#2425=CARTESIAN_POINT('Origin',(0.,58.18,1.3));
#2426=CARTESIAN_POINT('',(67.36,58.18,1.8));
#2427=CARTESIAN_POINT('',(0.,58.18,1.8));
#2428=CARTESIAN_POINT('',(16.84,58.18,1.8));
#2429=CARTESIAN_POINT('',(67.36,58.18,1.3));
#2430=CARTESIAN_POINT('',(67.36,58.18,0.65));
#2431=CARTESIAN_POINT('',(0.,58.18,1.3));
#2432=CARTESIAN_POINT('',(0.,58.18,1.3));
#2433=CARTESIAN_POINT('',(0.,58.18,0.65));
#2434=CARTESIAN_POINT('Origin',(67.36,58.82,1.3));
#2435=CARTESIAN_POINT('',(0.,58.82,1.8));
#2436=CARTESIAN_POINT('',(67.36,58.82,1.8));
#2437=CARTESIAN_POINT('',(50.52,58.82,1.8));
#2438=CARTESIAN_POINT('',(0.,58.82,1.3));
#2439=CARTESIAN_POINT('',(0.,58.82,0.65));
#2440=CARTESIAN_POINT('',(67.36,58.82,1.3));
#2441=CARTESIAN_POINT('',(67.36,58.82,1.3));
#2442=CARTESIAN_POINT('',(67.36,58.82,0.65));
#2443=CARTESIAN_POINT('Origin',(33.68,58.5,1.3));
#2444=CARTESIAN_POINT('',(0.,59.25,1.3));
#2445=CARTESIAN_POINT('',(67.36,29.25,1.3));
#2446=CARTESIAN_POINT('Origin',(67.36,0.,0.));
#2447=CARTESIAN_POINT('',(67.36,0.,1.8));
#2448=CARTESIAN_POINT('',(67.36,0.,1.8));
#2449=CARTESIAN_POINT('',(67.36,0.,0.));
#2450=CARTESIAN_POINT('',(67.36,0.,0.));
#2451=CARTESIAN_POINT('',(67.36,60.,0.));
#2452=CARTESIAN_POINT('',(67.36,0.,0.));
#2453=CARTESIAN_POINT('',(67.36,60.,1.8));
#2454=CARTESIAN_POINT('',(67.36,60.,0.));
#2455=CARTESIAN_POINT('',(67.36,0.,1.8));
#2456=CARTESIAN_POINT('Origin',(33.68,30.,1.8));
#2457=CARTESIAN_POINT('',(0.,0.,1.8));
#2458=CARTESIAN_POINT('',(0.,60.,1.8));
#2459=CARTESIAN_POINT('',(0.,0.,1.8));
#2460=CARTESIAN_POINT('Origin',(67.36,60.,0.));
#2461=CARTESIAN_POINT('',(0.,60.,0.));
#2462=CARTESIAN_POINT('',(67.36,60.,0.));
#2463=CARTESIAN_POINT('',(0.,60.,1.8));
#2464=CARTESIAN_POINT('',(0.,60.,0.));
#2465=CARTESIAN_POINT('',(67.36,60.,1.8));
#2466=CARTESIAN_POINT('Origin',(0.,0.,0.));
#2467=CARTESIAN_POINT('',(0.,0.,0.));
#2468=CARTESIAN_POINT('',(0.,0.,0.));
#2469=CARTESIAN_POINT('',(0.,0.,0.));
#2470=CARTESIAN_POINT('Origin',(0.,60.,0.));
#2471=CARTESIAN_POINT('',(0.,60.,1.8));
#2472=CARTESIAN_POINT('',(0.,60.,0.));
#2473=CARTESIAN_POINT('Origin',(33.68,30.,1.8));
#2474=CARTESIAN_POINT('Origin',(33.68,30.,0.));
#2475=CARTESIAN_POINT('',(0.,0.,0.));
#2476=CARTESIAN_POINT('Origin',(0.,58.18,1.3));
#2477=CARTESIAN_POINT('',(67.36,58.18,1.8));
#2478=CARTESIAN_POINT('',(0.,58.18,1.8));
#2479=CARTESIAN_POINT('',(16.84,58.18,1.8));
#2480=CARTESIAN_POINT('',(67.36,58.18,1.3));
#2481=CARTESIAN_POINT('',(67.36,58.18,0.65));
#2482=CARTESIAN_POINT('',(0.,58.18,1.3));
#2483=CARTESIAN_POINT('',(0.,58.18,1.3));
#2484=CARTESIAN_POINT('',(0.,58.18,0.65));
#2485=CARTESIAN_POINT('Origin',(67.36,58.82,1.3));
#2486=CARTESIAN_POINT('',(0.,58.82,1.8));
#2487=CARTESIAN_POINT('',(67.36,58.82,1.8));
#2488=CARTESIAN_POINT('',(50.52,58.82,1.8));
#2489=CARTESIAN_POINT('',(0.,58.82,1.3));
#2490=CARTESIAN_POINT('',(0.,58.82,0.65));
#2491=CARTESIAN_POINT('',(67.36,58.82,1.3));
#2492=CARTESIAN_POINT('',(67.36,58.82,1.3));
#2493=CARTESIAN_POINT('',(67.36,58.82,0.65));
#2494=CARTESIAN_POINT('Origin',(33.68,58.5,1.3));
#2495=CARTESIAN_POINT('',(0.,59.25,1.3));
#2496=CARTESIAN_POINT('',(67.36,29.25,1.3));
#2497=CARTESIAN_POINT('Origin',(67.36,0.,0.));
#2498=CARTESIAN_POINT('',(67.36,0.,1.8));
#2499=CARTESIAN_POINT('',(67.36,0.,1.8));
#2500=CARTESIAN_POINT('',(67.36,0.,0.));
#2501=CARTESIAN_POINT('',(67.36,0.,0.));
#2502=CARTESIAN_POINT('',(67.36,60.,0.));
#2503=CARTESIAN_POINT('',(67.36,0.,0.));
#2504=CARTESIAN_POINT('',(67.36,60.,1.8));
#2505=CARTESIAN_POINT('',(67.36,60.,0.));
#2506=CARTESIAN_POINT('',(67.36,0.,1.8));
#2507=CARTESIAN_POINT('Origin',(33.68,30.,1.8));
#2508=CARTESIAN_POINT('',(0.,0.,1.8));
#2509=CARTESIAN_POINT('',(0.,60.,1.8));
#2510=CARTESIAN_POINT('',(0.,0.,1.8));
#2511=CARTESIAN_POINT('Origin',(67.36,60.,0.));
#2512=CARTESIAN_POINT('',(0.,60.,0.));
#2513=CARTESIAN_POINT('',(67.36,60.,0.));
#2514=CARTESIAN_POINT('',(0.,60.,1.8));
#2515=CARTESIAN_POINT('',(0.,60.,0.));
#2516=CARTESIAN_POINT('',(67.36,60.,1.8));
#2517=CARTESIAN_POINT('Origin',(0.,0.,0.));
#2518=CARTESIAN_POINT('',(0.,0.,0.));
#2519=CARTESIAN_POINT('',(0.,0.,0.));
#2520=CARTESIAN_POINT('',(0.,0.,0.));
#2521=CARTESIAN_POINT('Origin',(0.,60.,0.));
#2522=CARTESIAN_POINT('',(0.,60.,1.8));
#2523=CARTESIAN_POINT('',(0.,60.,0.));
#2524=CARTESIAN_POINT('Origin',(33.68,30.,1.8));
#2525=CARTESIAN_POINT('Origin',(33.68,30.,0.));
#2526=CARTESIAN_POINT('',(0.,0.,0.));
#2527=CARTESIAN_POINT('Origin',(67.36,0.6,0.));
#2528=CARTESIAN_POINT('',(67.36,0.6,0.));
#2529=CARTESIAN_POINT('',(0.,0.6,0.));
#2530=CARTESIAN_POINT('',(67.36,0.6,0.));
#2531=CARTESIAN_POINT('',(0.,0.6,167.36));
#2532=CARTESIAN_POINT('',(0.,0.6,0.));
#2533=CARTESIAN_POINT('',(67.36,0.6,167.36));
#2534=CARTESIAN_POINT('',(67.36,0.6,167.36));
#2535=CARTESIAN_POINT('',(67.36,0.6,0.));
#2536=CARTESIAN_POINT('Origin',(67.36,0.,0.));
#2537=CARTESIAN_POINT('',(67.36,0.,0.));
#2538=CARTESIAN_POINT('',(67.36,0.,0.));
#2539=CARTESIAN_POINT('',(67.36,0.,167.36));
#2540=CARTESIAN_POINT('',(67.36,0.,167.36));
#2541=CARTESIAN_POINT('',(67.36,0.,0.));
#2542=CARTESIAN_POINT('Origin',(0.,0.,0.));
#2543=CARTESIAN_POINT('',(0.,0.,0.));
#2544=CARTESIAN_POINT('',(0.,0.,0.));
#2545=CARTESIAN_POINT('',(0.,0.,167.36));
#2546=CARTESIAN_POINT('',(0.,0.,167.36));
#2547=CARTESIAN_POINT('',(0.,0.,0.));
#2548=CARTESIAN_POINT('Origin',(0.,0.6,0.));
#2549=CARTESIAN_POINT('',(0.,0.6,0.));
#2550=CARTESIAN_POINT('',(0.,0.6,167.36));
#2551=CARTESIAN_POINT('Origin',(33.68,0.3,167.36));
#2552=CARTESIAN_POINT('Origin',(33.68,0.3,0.));
#2553=CARTESIAN_POINT('',(0.,0.,0.));
#2554=CARTESIAN_POINT('Origin',(67.36,57.6,0.));
#2555=CARTESIAN_POINT('',(67.36,57.6,0.));
#2556=CARTESIAN_POINT('',(0.,57.6,0.));
#2557=CARTESIAN_POINT('',(67.36,57.6,0.));
#2558=CARTESIAN_POINT('',(0.,57.6,1.8));
#2559=CARTESIAN_POINT('',(0.,57.6,0.));
#2560=CARTESIAN_POINT('',(67.36,57.6,1.8));
#2561=CARTESIAN_POINT('',(67.36,57.6,1.8));
#2562=CARTESIAN_POINT('',(67.36,57.6,0.));
#2563=CARTESIAN_POINT('Origin',(67.36,0.6,0.));
#2564=CARTESIAN_POINT('',(67.36,0.6,0.));
#2565=CARTESIAN_POINT('',(67.36,0.6,0.));
#2566=CARTESIAN_POINT('',(67.36,0.600000000000001,1.8));
#2567=CARTESIAN_POINT('',(67.36,0.6,1.8));
#2568=CARTESIAN_POINT('',(67.36,0.6,0.));
#2569=CARTESIAN_POINT('Origin',(0.,0.6,0.));
#2570=CARTESIAN_POINT('',(0.,0.600000000000001,0.));
#2571=CARTESIAN_POINT('',(0.,0.6,0.));
#2572=CARTESIAN_POINT('',(0.,0.600000000000001,1.8));
#2573=CARTESIAN_POINT('',(0.,0.6,1.8));
#2574=CARTESIAN_POINT('',(0.,0.600000000000001,0.));
#2575=CARTESIAN_POINT('Origin',(0.,57.6,0.));
#2576=CARTESIAN_POINT('',(0.,57.6,0.));
#2577=CARTESIAN_POINT('',(0.,57.6,1.8));
#2578=CARTESIAN_POINT('Origin',(33.68,29.1,1.8));
#2579=CARTESIAN_POINT('Origin',(33.68,29.1,0.));
#2580=CARTESIAN_POINT('',(0.,0.,0.));
#2581=CARTESIAN_POINT('Origin',(0.,0.,66.36));
#2582=CARTESIAN_POINT('',(-0.6,-7.34788079488412E-17,66.96));
#2583=CARTESIAN_POINT('Origin',(0.,0.,66.96));
#2584=CARTESIAN_POINT('',(-0.6,-7.34788079488412E-17,66.36));
#2585=CARTESIAN_POINT('',(-0.6,-7.34788079488412E-17,66.36));
#2586=CARTESIAN_POINT('Origin',(0.,0.,66.36));
#2587=CARTESIAN_POINT('Origin',(0.,0.,66.96));
#2588=CARTESIAN_POINT('Origin',(0.,0.,-0.6));
#2589=CARTESIAN_POINT('',(-0.6,-7.34788079488412E-17,0.));
#2590=CARTESIAN_POINT('Origin',(0.,0.,0.));
#2591=CARTESIAN_POINT('',(-0.6,-7.34788079488412E-17,-0.6));
#2592=CARTESIAN_POINT('',(-0.6,-7.34788079488412E-17,-0.6));
#2593=CARTESIAN_POINT('Origin',(0.,0.,-0.6));
#2594=CARTESIAN_POINT('Origin',(0.,0.,-0.6));
#2595=CARTESIAN_POINT('Origin',(0.,0.,0.));
#2596=CARTESIAN_POINT('',(-1.25,-1.53080849893419E-16,66.36));
#2597=CARTESIAN_POINT('Origin',(0.,0.,66.36));
#2598=CARTESIAN_POINT('',(-1.25,-1.53080849893419E-16,0.));
#2599=CARTESIAN_POINT('',(-1.25,-1.53080849893419E-16,0.));
#2600=CARTESIAN_POINT('Origin',(0.,0.,0.));
#2601=CARTESIAN_POINT('Origin',(0.,0.,66.36));
#2602=CARTESIAN_POINT('Origin',(0.,0.,0.));
#2603=CARTESIAN_POINT('',(0.,0.,0.));
#2604=CARTESIAN_POINT('Origin',(0.,0.,10.));
#2605=CARTESIAN_POINT('',(-0.6,-7.34788079488412E-17,11.));
#2606=CARTESIAN_POINT('Origin',(0.,0.,11.));
#2607=CARTESIAN_POINT('',(-0.6,-7.34788079488412E-17,10.));
#2608=CARTESIAN_POINT('',(-0.6,-7.34788079488412E-17,10.));
#2609=CARTESIAN_POINT('Origin',(0.,0.,10.));
#2610=CARTESIAN_POINT('Origin',(0.,0.,11.));
#2611=CARTESIAN_POINT('Origin',(0.,0.,0.));
#2612=CARTESIAN_POINT('',(-5.,-6.12323399573677E-16,10.));
#2613=CARTESIAN_POINT('Origin',(0.,0.,10.));
#2614=CARTESIAN_POINT('',(-5.,-6.12323399573677E-16,0.));
#2615=CARTESIAN_POINT('',(-5.,-6.12323399573677E-16,0.));
#2616=CARTESIAN_POINT('Origin',(0.,0.,0.));
#2617=CARTESIAN_POINT('Origin',(0.,0.,10.));
#2618=CARTESIAN_POINT('Origin',(0.,0.,0.));
#2619=CARTESIAN_POINT('',(0.,0.,0.));
#2620=CARTESIAN_POINT('Origin',(0.,0.,0.));
#2621=CARTESIAN_POINT('',(-0.4,-4.89858719658941E-17,2.8));
#2622=CARTESIAN_POINT('Origin',(0.,0.,2.8));
#2623=CARTESIAN_POINT('',(-0.4,-4.89858719658941E-17,0.));
#2624=CARTESIAN_POINT('',(-0.4,-4.89858719658941E-17,0.));
#2625=CARTESIAN_POINT('Origin',(0.,0.,0.));
#2626=CARTESIAN_POINT('Origin',(0.,0.,2.8));
#2627=CARTESIAN_POINT('Origin',(0.,0.,0.));
#2628=CARTESIAN_POINT('',(0.,0.,10.));
#2629=CARTESIAN_POINT('',(1.32,0.,10.));
#2630=CARTESIAN_POINT('',(68.68,0.,180.));
#2631=CARTESIAN_POINT('',(1.32,58.2,11.32));
#2632=CARTESIAN_POINT('',(1.32,0.,94.1));
#2633=CARTESIAN_POINT('',(1.82,30.,162.));
#2634=CARTESIAN_POINT('',(6.5,6.5,0.));
#2635=CARTESIAN_POINT('',(68.6,9.,66.7));
#2636=CARTESIAN_POINT('',(70.,0.,180.));
#2637=CARTESIAN_POINT('',(6.5,53.5,0.));
#2638=CARTESIAN_POINT('',(63.5,6.5,0.));
#2639=CARTESIAN_POINT('',(63.5,53.5,0.));
#2640=CARTESIAN_POINT('',(70.,0.,10.));
#2641=CARTESIAN_POINT('',(140.,0.,180.));
#2642=CARTESIAN_POINT('',(71.32,0.,10.));
#2643=CARTESIAN_POINT('',(138.68,0.,180.));
#2644=CARTESIAN_POINT('',(71.32,58.2,11.32));
#2645=CARTESIAN_POINT('',(71.32,0.,94.1));
#2646=CARTESIAN_POINT('',(71.82,30.,162.));
#2647=CARTESIAN_POINT('',(76.5,6.5,0.));
#2648=CARTESIAN_POINT('',(76.5,53.5,0.));
#2649=CARTESIAN_POINT('',(133.5,6.5,0.));
#2650=CARTESIAN_POINT('',(133.5,53.5,0.));
#2651=CARTESIAN_POINT('',(68.6,9.,123.3));
#2652=CARTESIAN_POINT('',(68.6,51.,66.7));
#2653=CARTESIAN_POINT('',(68.6,51.,123.3));
#2654=UNCERTAINTY_MEASURE_WITH_UNIT(LENGTH_MEASURE(0.001),#2674,
'DISTANCE_ACCURACY_VALUE',
'Maximum model space distance between geometric entities at asserted c
onnectivities');
#2655=UNCERTAINTY_MEASURE_WITH_UNIT(LENGTH_MEASURE(0.001),#2674,
'DISTANCE_ACCURACY_VALUE',
'Maximum model space distance between geometric entities at asserted c
onnectivities');
#2656=UNCERTAINTY_MEASURE_WITH_UNIT(LENGTH_MEASURE(0.001),#2674,
'DISTANCE_ACCURACY_VALUE',
'Maximum model space distance between geometric entities at asserted c
onnectivities');
#2657=UNCERTAINTY_MEASURE_WITH_UNIT(LENGTH_MEASURE(0.001),#2674,
'DISTANCE_ACCURACY_VALUE',
'Maximum model space distance between geometric entities at asserted c
onnectivities');
#2658=UNCERTAINTY_MEASURE_WITH_UNIT(LENGTH_MEASURE(0.001),#2674,
'DISTANCE_ACCURACY_VALUE',
'Maximum model space distance between geometric entities at asserted c
onnectivities');
#2659=UNCERTAINTY_MEASURE_WITH_UNIT(LENGTH_MEASURE(0.001),#2674,
'DISTANCE_ACCURACY_VALUE',
'Maximum model space distance between geometric entities at asserted c
onnectivities');
#2660=UNCERTAINTY_MEASURE_WITH_UNIT(LENGTH_MEASURE(0.001),#2674,
'DISTANCE_ACCURACY_VALUE',
'Maximum model space distance between geometric entities at asserted c
onnectivities');
#2661=UNCERTAINTY_MEASURE_WITH_UNIT(LENGTH_MEASURE(0.001),#2674,
'DISTANCE_ACCURACY_VALUE',
'Maximum model space distance between geometric entities at asserted c
onnectivities');
#2662=UNCERTAINTY_MEASURE_WITH_UNIT(LENGTH_MEASURE(0.001),#2674,
'DISTANCE_ACCURACY_VALUE',
'Maximum model space distance between geometric entities at asserted c
onnectivities');
#2663=UNCERTAINTY_MEASURE_WITH_UNIT(LENGTH_MEASURE(0.001),#2674,
'DISTANCE_ACCURACY_VALUE',
'Maximum model space distance between geometric entities at asserted c
onnectivities');
#2664=(
GEOMETRIC_REPRESENTATION_CONTEXT(3)
GLOBAL_UNCERTAINTY_ASSIGNED_CONTEXT((#2654))
GLOBAL_UNIT_ASSIGNED_CONTEXT((#2674,#2676,#2677))
REPRESENTATION_CONTEXT('','3D')
);
#2665=(
GEOMETRIC_REPRESENTATION_CONTEXT(3)
GLOBAL_UNCERTAINTY_ASSIGNED_CONTEXT((#2655))
GLOBAL_UNIT_ASSIGNED_CONTEXT((#2674,#2676,#2677))
REPRESENTATION_CONTEXT('','3D')
);
#2666=(
GEOMETRIC_REPRESENTATION_CONTEXT(3)
GLOBAL_UNCERTAINTY_ASSIGNED_CONTEXT((#2656))
GLOBAL_UNIT_ASSIGNED_CONTEXT((#2674,#2676,#2677))
REPRESENTATION_CONTEXT('','3D')
);
#2667=(
GEOMETRIC_REPRESENTATION_CONTEXT(3)
GLOBAL_UNCERTAINTY_ASSIGNED_CONTEXT((#2657))
GLOBAL_UNIT_ASSIGNED_CONTEXT((#2674,#2676,#2677))
REPRESENTATION_CONTEXT('','3D')
);
#2668=(
GEOMETRIC_REPRESENTATION_CONTEXT(3)
GLOBAL_UNCERTAINTY_ASSIGNED_CONTEXT((#2658))
GLOBAL_UNIT_ASSIGNED_CONTEXT((#2674,#2676,#2677))
REPRESENTATION_CONTEXT('','3D')
);
#2669=(
GEOMETRIC_REPRESENTATION_CONTEXT(3)
GLOBAL_UNCERTAINTY_ASSIGNED_CONTEXT((#2659))
GLOBAL_UNIT_ASSIGNED_CONTEXT((#2674,#2676,#2677))
REPRESENTATION_CONTEXT('','3D')
);
#2670=(
GEOMETRIC_REPRESENTATION_CONTEXT(3)
GLOBAL_UNCERTAINTY_ASSIGNED_CONTEXT((#2660))
GLOBAL_UNIT_ASSIGNED_CONTEXT((#2674,#2676,#2677))
REPRESENTATION_CONTEXT('','3D')
);
#2671=(
GEOMETRIC_REPRESENTATION_CONTEXT(3)
GLOBAL_UNCERTAINTY_ASSIGNED_CONTEXT((#2661))
GLOBAL_UNIT_ASSIGNED_CONTEXT((#2674,#2676,#2677))
REPRESENTATION_CONTEXT('','3D')
);
#2672=(
GEOMETRIC_REPRESENTATION_CONTEXT(3)
GLOBAL_UNCERTAINTY_ASSIGNED_CONTEXT((#2662))
GLOBAL_UNIT_ASSIGNED_CONTEXT((#2674,#2676,#2677))
REPRESENTATION_CONTEXT('','3D')
);
#2673=(
GEOMETRIC_REPRESENTATION_CONTEXT(3)
GLOBAL_UNCERTAINTY_ASSIGNED_CONTEXT((#2663))
GLOBAL_UNIT_ASSIGNED_CONTEXT((#2674,#2676,#2677))
REPRESENTATION_CONTEXT('','3D')
);
#2674=(
LENGTH_UNIT()
NAMED_UNIT(*)
SI_UNIT(.CENTI.,.METRE.)
);
#2675=(
LENGTH_UNIT()
NAMED_UNIT(*)
SI_UNIT($,.METRE.)
);
#2676=(
NAMED_UNIT(*)
PLANE_ANGLE_UNIT()
SI_UNIT($,.RADIAN.)
);
#2677=(
NAMED_UNIT(*)
SI_UNIT($,.STERADIAN.)
SOLID_ANGLE_UNIT()
);
#2678=SHAPE_DEFINITION_REPRESENTATION(#2687,#2722);
#2679=SHAPE_DEFINITION_REPRESENTATION(#2688,#2723);
#2680=SHAPE_DEFINITION_REPRESENTATION(#2689,#2724);
#2681=SHAPE_DEFINITION_REPRESENTATION(#2690,#2725);
#2682=SHAPE_DEFINITION_REPRESENTATION(#2691,#2726);
#2683=SHAPE_DEFINITION_REPRESENTATION(#2692,#2727);
#2684=SHAPE_DEFINITION_REPRESENTATION(#2693,#2728);
#2685=SHAPE_DEFINITION_REPRESENTATION(#2694,#2729);
#2686=SHAPE_DEFINITION_REPRESENTATION(#2695,#2730);
#2687=PRODUCT_DEFINITION_SHAPE('',$,#2732);
#2688=PRODUCT_DEFINITION_SHAPE('',$,#2733);
#2689=PRODUCT_DEFINITION_SHAPE('',$,#2734);
#2690=PRODUCT_DEFINITION_SHAPE('',$,#2735);
#2691=PRODUCT_DEFINITION_SHAPE('',$,#2736);
#2692=PRODUCT_DEFINITION_SHAPE('',$,#2737);
#2693=PRODUCT_DEFINITION_SHAPE('',$,#2738);
#2694=PRODUCT_DEFINITION_SHAPE('',$,#2739);
#2695=PRODUCT_DEFINITION_SHAPE('',$,#2740);
#2696=PRODUCT_DEFINITION_SHAPE($,$,#89);
#2697=PRODUCT_DEFINITION_SHAPE($,$,#90);
#2698=PRODUCT_DEFINITION_SHAPE($,$,#91);
#2699=PRODUCT_DEFINITION_SHAPE($,$,#92);
#2700=PRODUCT_DEFINITION_SHAPE($,$,#93);
#2701=PRODUCT_DEFINITION_SHAPE($,$,#94);
#2702=PRODUCT_DEFINITION_SHAPE($,$,#95);
#2703=PRODUCT_DEFINITION_SHAPE($,$,#96);
#2704=PRODUCT_DEFINITION_SHAPE($,$,#97);
#2705=PRODUCT_DEFINITION_SHAPE($,$,#98);
#2706=PRODUCT_DEFINITION_SHAPE($,$,#99);
#2707=PRODUCT_DEFINITION_SHAPE($,$,#100);
#2708=PRODUCT_DEFINITION_SHAPE($,$,#101);
#2709=PRODUCT_DEFINITION_SHAPE($,$,#102);
#2710=PRODUCT_DEFINITION_SHAPE($,$,#103);
#2711=PRODUCT_DEFINITION_SHAPE($,$,#104);
#2712=PRODUCT_DEFINITION_SHAPE($,$,#105);
#2713=PRODUCT_DEFINITION_SHAPE($,$,#106);
#2714=PRODUCT_DEFINITION_SHAPE($,$,#107);
#2715=PRODUCT_DEFINITION_SHAPE($,$,#108);
#2716=PRODUCT_DEFINITION_SHAPE($,$,#109);
#2717=PRODUCT_DEFINITION_SHAPE($,$,#110);
#2718=PRODUCT_DEFINITION_SHAPE($,$,#111);
#2719=PRODUCT_DEFINITION_SHAPE($,$,#112);
#2720=PRODUCT_DEFINITION_SHAPE($,$,#113);
#2721=PRODUCT_DEFINITION_SHAPE($,$,#114);
#2722=SHAPE_REPRESENTATION('',(#1614,#1744,#1745,#1746,#1747,#1748,#1749,
#1750,#1751,#1752,#1753,#1754,#1755,#1756,#1757,#1758,#1759,#1760,#1761,
#1762,#1763,#1764,#1765,#1766,#1767,#1768,#1769),#2664);
#2723=SHAPE_REPRESENTATION('',(#1615),#2665);
#2724=SHAPE_REPRESENTATION('',(#1662),#2666);
#2725=SHAPE_REPRESENTATION('',(#1689),#2667);
#2726=SHAPE_REPRESENTATION('',(#1700),#2668);
#2727=SHAPE_REPRESENTATION('',(#1707),#2669);
#2728=SHAPE_REPRESENTATION('',(#1714),#2670);
#2729=SHAPE_REPRESENTATION('',(#1728),#2671);
#2730=SHAPE_REPRESENTATION('',(#1738),#2672);
#2731=PRODUCT_DEFINITION_CONTEXT('part definition',#2760,'design');
#2732=PRODUCT_DEFINITION('TAS-024','TAS-024',#2741,#2731);
#2733=PRODUCT_DEFINITION('Universal side panel','Universal side panel',
#2742,#2731);
#2734=PRODUCT_DEFINITION('Foot socket base panel',
'Foot socket base panel',#2743,#2731);
#2735=PRODUCT_DEFINITION('Top Panel','Top panel',#2744,#2731);
#2736=PRODUCT_DEFINITION('Captured back panel','Captured back panel',#2745,
#2731);
#2737=PRODUCT_DEFINITION('Fixed shelf','Fixed shelf',#2746,#2731);
#2738=PRODUCT_DEFINITION('Hanging rail','Hanging rail',#2747,#2731);
#2739=PRODUCT_DEFINITION('Turned support foot','Turned support foot',#2748,
#2731);
#2740=PRODUCT_DEFINITION('Bay coupling dowel','Bay coupling dowel',#2749,
#2731);
#2741=PRODUCT_DEFINITION_FORMATION('',$,#2762);
#2742=PRODUCT_DEFINITION_FORMATION('',$,#2763);
#2743=PRODUCT_DEFINITION_FORMATION('',$,#2764);
#2744=PRODUCT_DEFINITION_FORMATION('',$,#2765);
#2745=PRODUCT_DEFINITION_FORMATION('',$,#2766);
#2746=PRODUCT_DEFINITION_FORMATION('',$,#2767);
#2747=PRODUCT_DEFINITION_FORMATION('',$,#2768);
#2748=PRODUCT_DEFINITION_FORMATION('',$,#2769);
#2749=PRODUCT_DEFINITION_FORMATION('',$,#2770);
#2750=PRODUCT_RELATED_PRODUCT_CATEGORY('TAS-024','TAS-024',(#2762));
#2751=PRODUCT_RELATED_PRODUCT_CATEGORY('Universal side panel',
'Universal side panel',(#2763));
#2752=PRODUCT_RELATED_PRODUCT_CATEGORY('Foot socket base panel',
'Foot socket base panel',(#2764));
#2753=PRODUCT_RELATED_PRODUCT_CATEGORY('Top panel','Top panel',(#2765));
#2754=PRODUCT_RELATED_PRODUCT_CATEGORY('Captured back panel',
'Captured back panel',(#2766));
#2755=PRODUCT_RELATED_PRODUCT_CATEGORY('Fixed shelf','Fixed shelf',(#2767));
#2756=PRODUCT_RELATED_PRODUCT_CATEGORY('Hanging rail','Hanging rail',(#2768));
#2757=PRODUCT_RELATED_PRODUCT_CATEGORY('Turned support foot',
'Turned support foot',(#2769));
#2758=PRODUCT_RELATED_PRODUCT_CATEGORY('Bay coupling dowel',
'Bay coupling dowel',(#2770));
#2759=APPLICATION_PROTOCOL_DEFINITION('international standard',
'automotive_design',2009,#2760);
#2760=APPLICATION_CONTEXT(
'Core Data for Automotive Mechanical Design Process');
#2761=PRODUCT_CONTEXT('part definition',#2760,'mechanical');
#2762=PRODUCT('TAS-024','TAS-024',$,(#2761));
#2763=PRODUCT('Universal side panel','Universal side panel',$,(#2761));
#2764=PRODUCT('Foot socket base panel','Foot socket base panel',$,(#2761));
#2765=PRODUCT('Top Panel','Top panel',$,(#2761));
#2766=PRODUCT('Captured back panel','Captured back panel',$,(#2761));
#2767=PRODUCT('Fixed shelf','Fixed shelf',$,(#2761));
#2768=PRODUCT('Hanging rail','Hanging rail',$,(#2761));
#2769=PRODUCT('Turned support foot','Turned support foot',$,(#2761));
#2770=PRODUCT('Bay coupling dowel','Bay coupling dowel',$,(#2761));
#2771=PRESENTATION_STYLE_ASSIGNMENT((#2780));
#2772=PRESENTATION_STYLE_ASSIGNMENT((#2781));
#2773=PRESENTATION_STYLE_ASSIGNMENT((#2782));
#2774=PRESENTATION_STYLE_ASSIGNMENT((#2783));
#2775=PRESENTATION_STYLE_ASSIGNMENT((#2784));
#2776=PRESENTATION_STYLE_ASSIGNMENT((#2785));
#2777=PRESENTATION_STYLE_ASSIGNMENT((#2786));
#2778=PRESENTATION_STYLE_ASSIGNMENT((#2787));
#2779=PRESENTATION_STYLE_ASSIGNMENT((#2788));
#2780=SURFACE_STYLE_USAGE(.BOTH.,#2789);
#2781=SURFACE_STYLE_USAGE(.BOTH.,#2790);
#2782=SURFACE_STYLE_USAGE(.BOTH.,#2791);
#2783=SURFACE_STYLE_USAGE(.BOTH.,#2792);
#2784=SURFACE_STYLE_USAGE(.BOTH.,#2793);
#2785=SURFACE_STYLE_USAGE(.BOTH.,#2794);
#2786=SURFACE_STYLE_USAGE(.BOTH.,#2795);
#2787=SURFACE_STYLE_USAGE(.BOTH.,#2796);
#2788=SURFACE_STYLE_USAGE(.BOTH.,#2797);
#2789=SURFACE_SIDE_STYLE('',(#2798));
#2790=SURFACE_SIDE_STYLE('',(#2799));
#2791=SURFACE_SIDE_STYLE('',(#2800));
#2792=SURFACE_SIDE_STYLE('',(#2801));
#2793=SURFACE_SIDE_STYLE('',(#2802));
#2794=SURFACE_SIDE_STYLE('',(#2803));
#2795=SURFACE_SIDE_STYLE('',(#2804));
#2796=SURFACE_SIDE_STYLE('',(#2805));
#2797=SURFACE_SIDE_STYLE('',(#2806));
#2798=SURFACE_STYLE_FILL_AREA(#2807);
#2799=SURFACE_STYLE_FILL_AREA(#2808);
#2800=SURFACE_STYLE_FILL_AREA(#2809);
#2801=SURFACE_STYLE_FILL_AREA(#2810);
#2802=SURFACE_STYLE_FILL_AREA(#2811);
#2803=SURFACE_STYLE_FILL_AREA(#2812);
#2804=SURFACE_STYLE_FILL_AREA(#2813);
#2805=SURFACE_STYLE_FILL_AREA(#2814);
#2806=SURFACE_STYLE_FILL_AREA(#2815);
#2807=FILL_AREA_STYLE('Steel - Satin',(#2816));
#2808=FILL_AREA_STYLE('Universal side panel finish',(#2817));
#2809=FILL_AREA_STYLE('Foot socket base panel finish',(#2818));
#2810=FILL_AREA_STYLE('Top panel finish',(#2819));
#2811=FILL_AREA_STYLE('Captured back panel finish',(#2820));
#2812=FILL_AREA_STYLE('Fixed shelf finish',(#2821));
#2813=FILL_AREA_STYLE('Hanging rail finish',(#2822));
#2814=FILL_AREA_STYLE('Turned support foot finish',(#2823));
#2815=FILL_AREA_STYLE('Bay coupling dowel finish',(#2824));
#2816=FILL_AREA_STYLE_COLOUR('Steel - Satin',#2825);
#2817=FILL_AREA_STYLE_COLOUR('Universal side panel finish',#2826);
#2818=FILL_AREA_STYLE_COLOUR('Foot socket base panel finish',#2827);
#2819=FILL_AREA_STYLE_COLOUR('Top panel finish',#2828);
#2820=FILL_AREA_STYLE_COLOUR('Captured back panel finish',#2829);
#2821=FILL_AREA_STYLE_COLOUR('Fixed shelf finish',#2830);
#2822=FILL_AREA_STYLE_COLOUR('Hanging rail finish',#2831);
#2823=FILL_AREA_STYLE_COLOUR('Turned support foot finish',#2832);
#2824=FILL_AREA_STYLE_COLOUR('Bay coupling dowel finish',#2833);
#2825=COLOUR_RGB('Steel - Satin',0.627450980392157,0.627450980392157,0.627450980392157);
#2826=COLOUR_RGB('Universal side panel finish',0.0941176470588235,0.231372549019608,
0.431372549019608);
#2827=COLOUR_RGB('Foot socket base panel finish',0.662745098039216,0.823529411764706,
0.917647058823529);
#2828=COLOUR_RGB('Top panel finish',0.662745098039216,0.823529411764706,
0.917647058823529);
#2829=COLOUR_RGB('Captured back panel finish',0.607843137254902,0.647058823529412,
0.701960784313725);
#2830=COLOUR_RGB('Fixed shelf finish',0.274509803921569,0.6,0.8);
#2831=COLOUR_RGB('Hanging rail finish',0.607843137254902,0.647058823529412,
0.701960784313725);
#2832=COLOUR_RGB('Turned support foot finish',0.188235294117647,0.211764705882353,
0.247058823529412);
#2833=COLOUR_RGB('Bay coupling dowel finish',0.43921568627451,0.47843137254902,
0.52156862745098);
ENDSEC;
END-ISO-10303-21;
